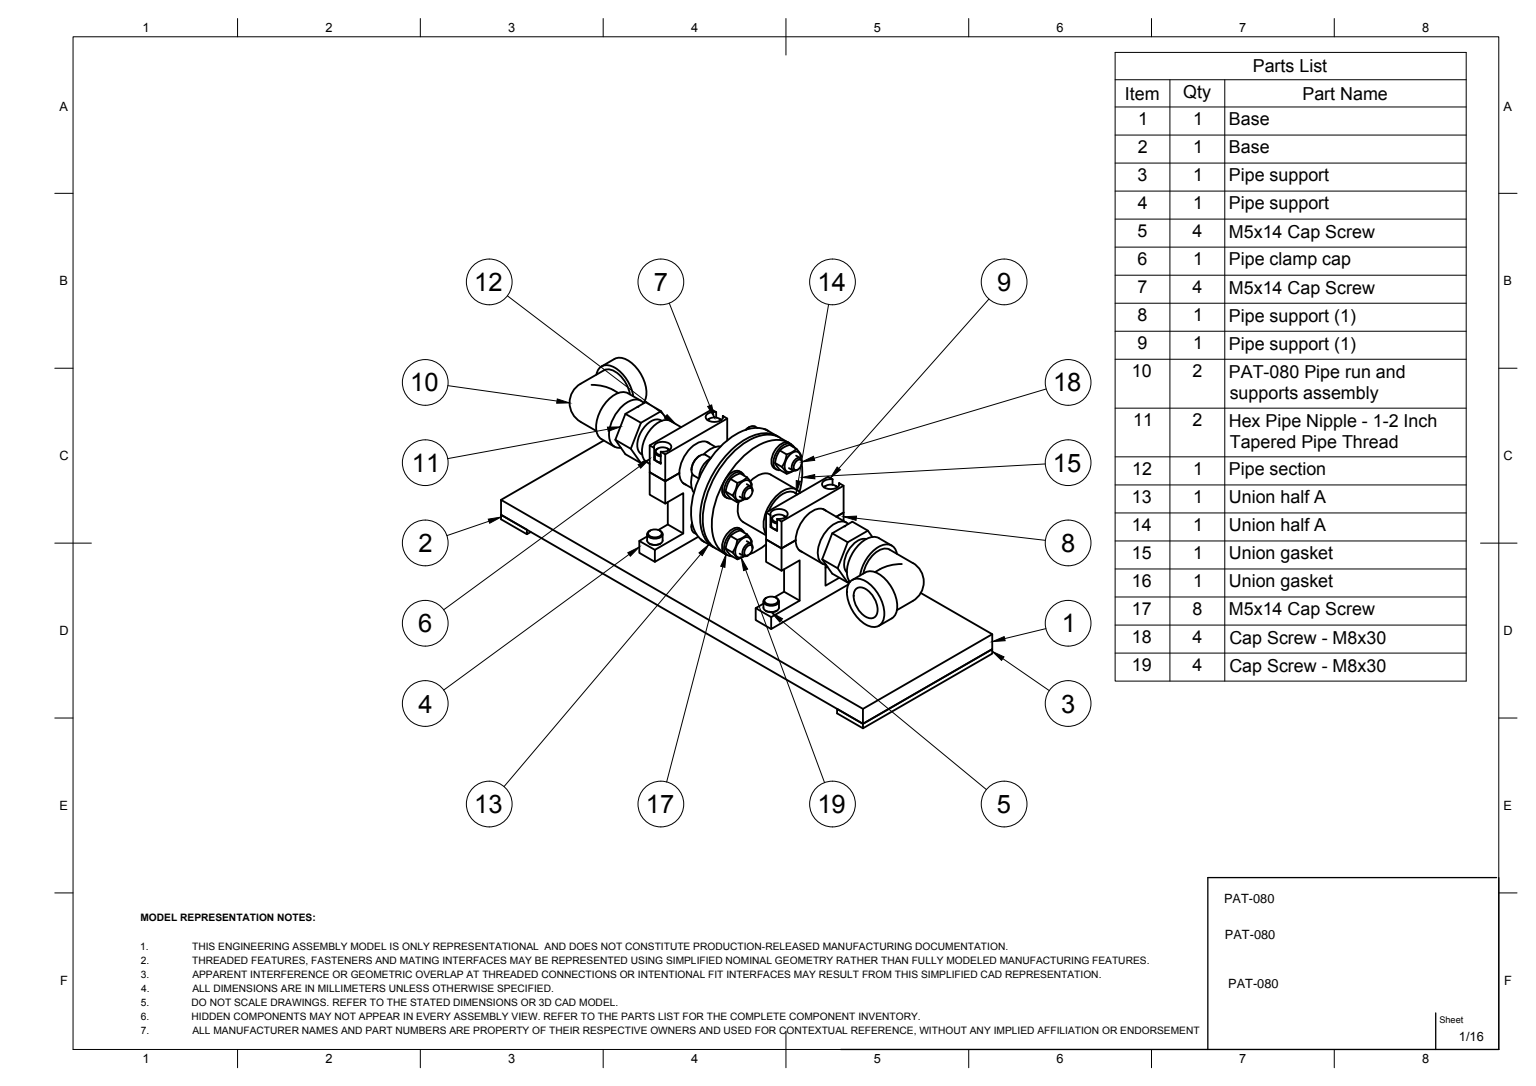
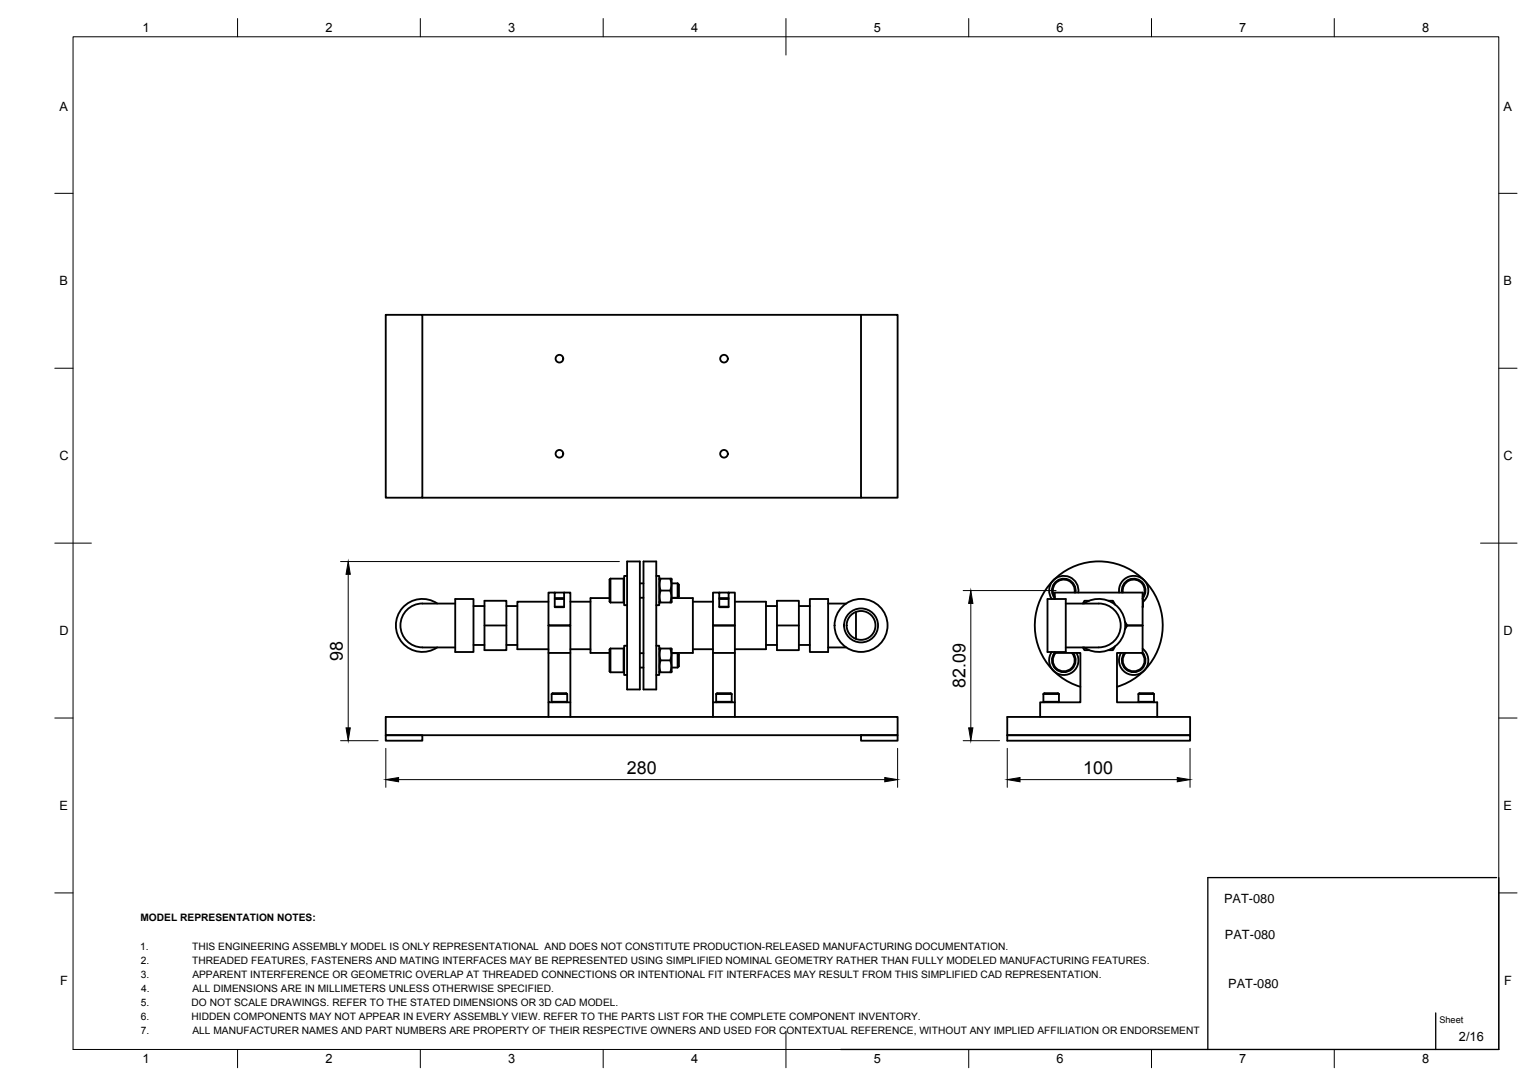
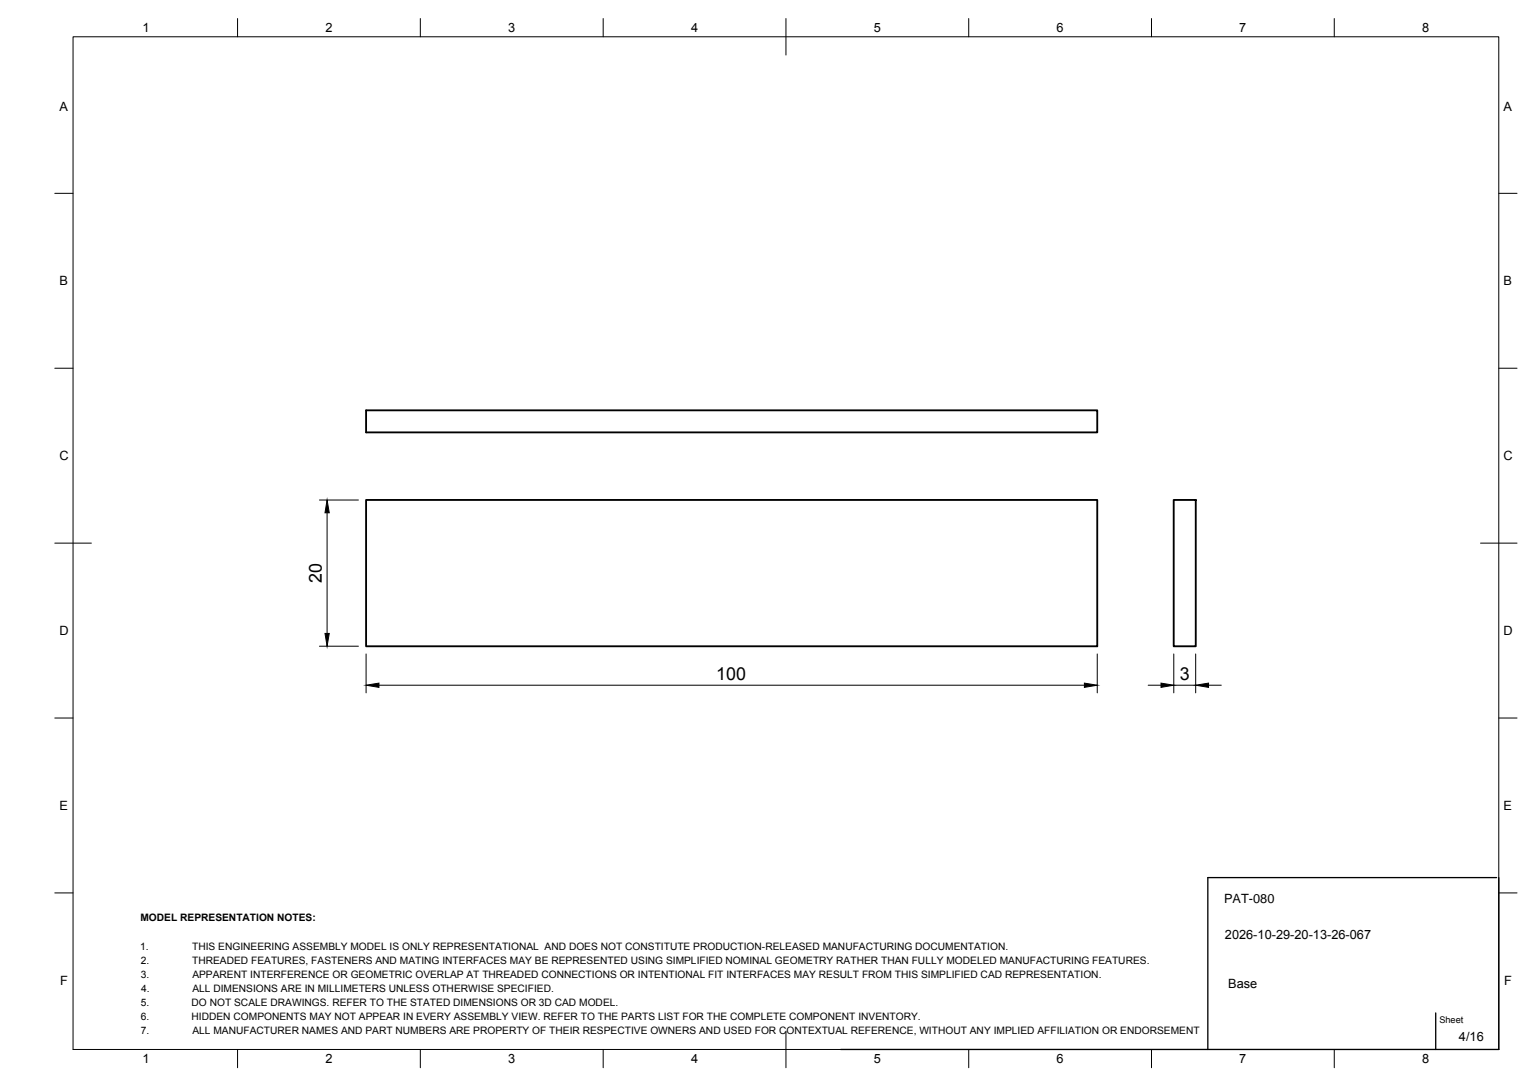
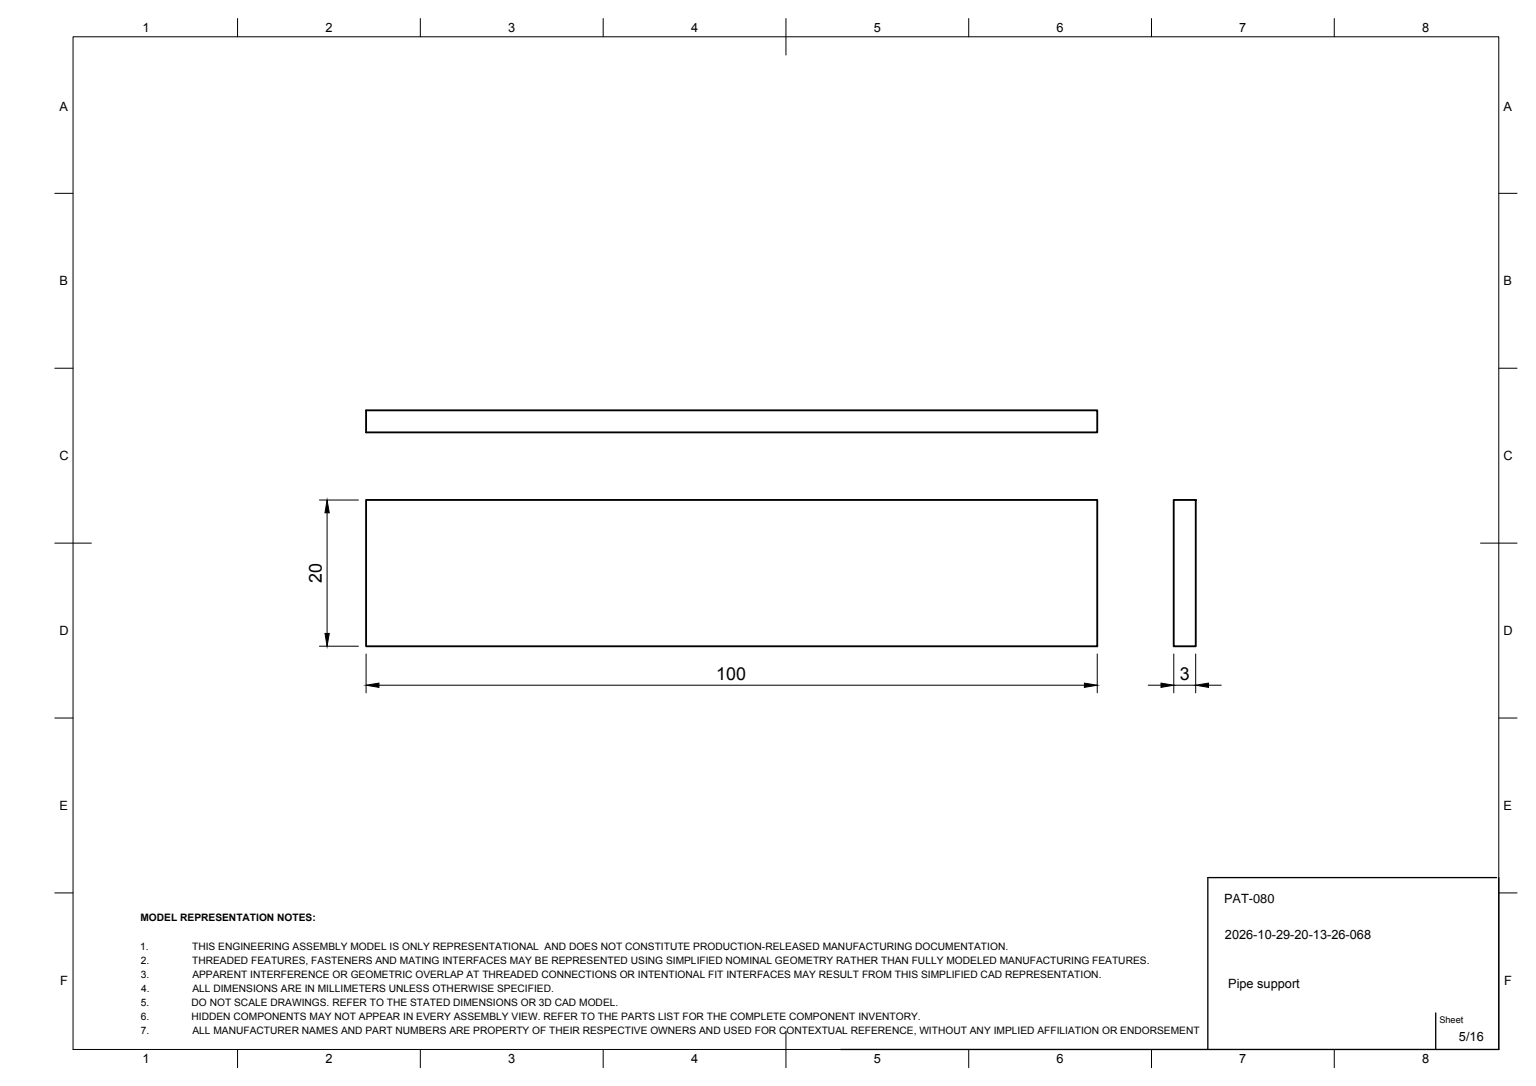
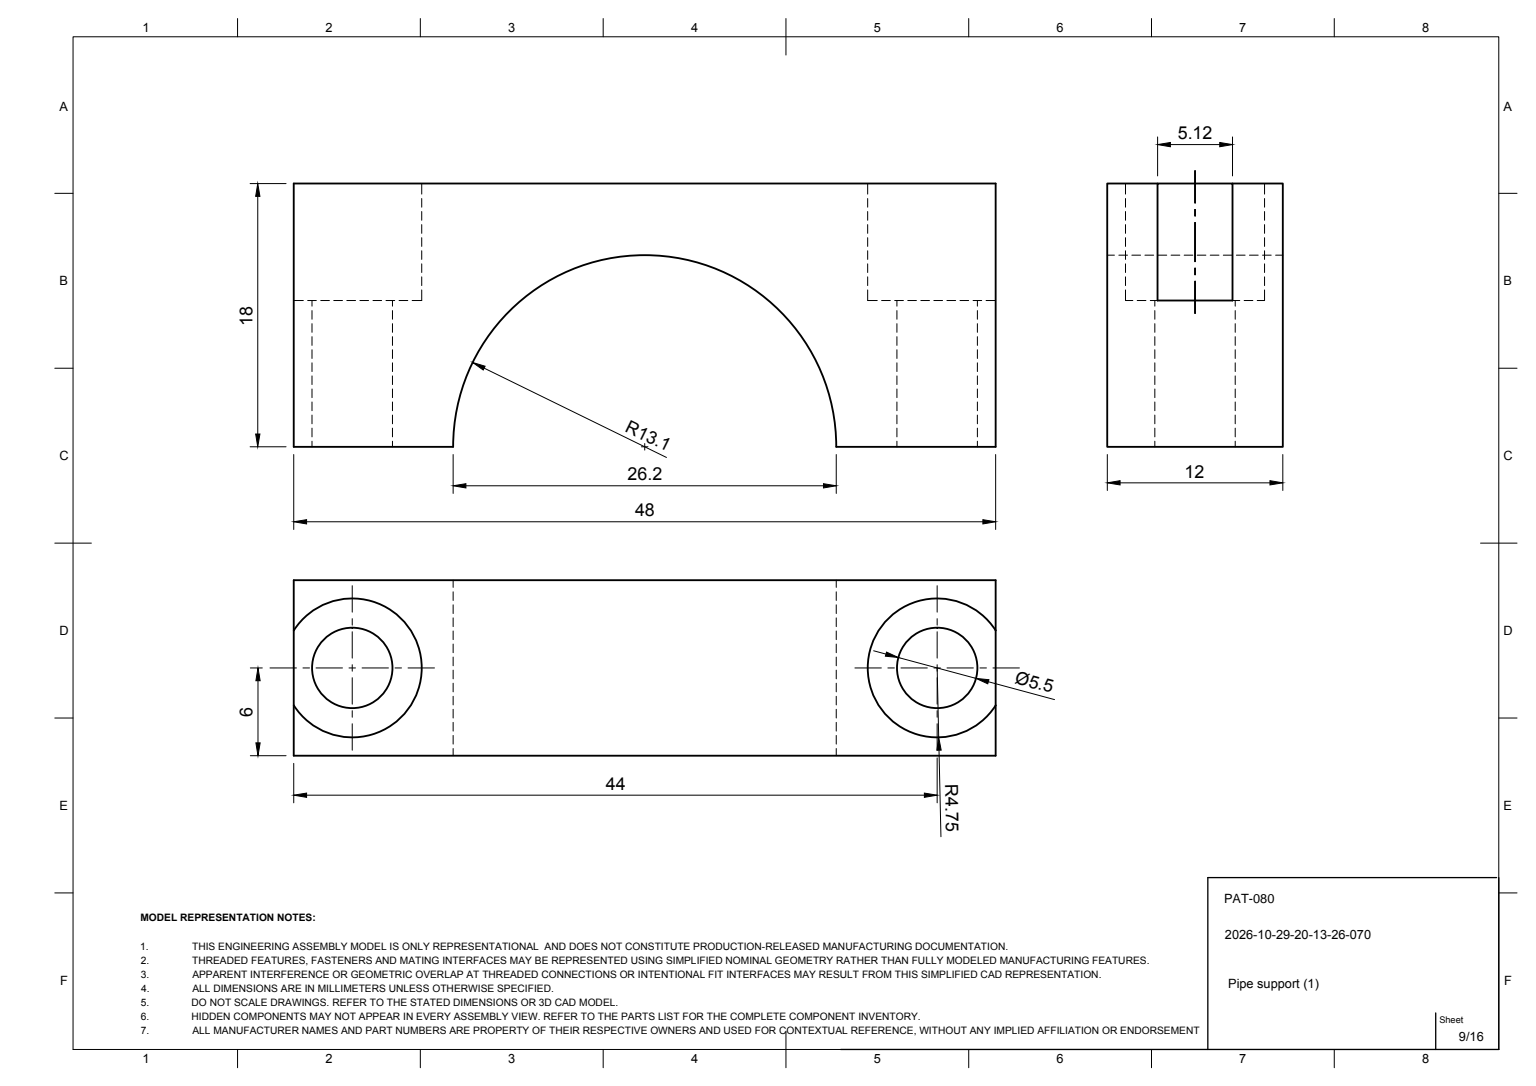
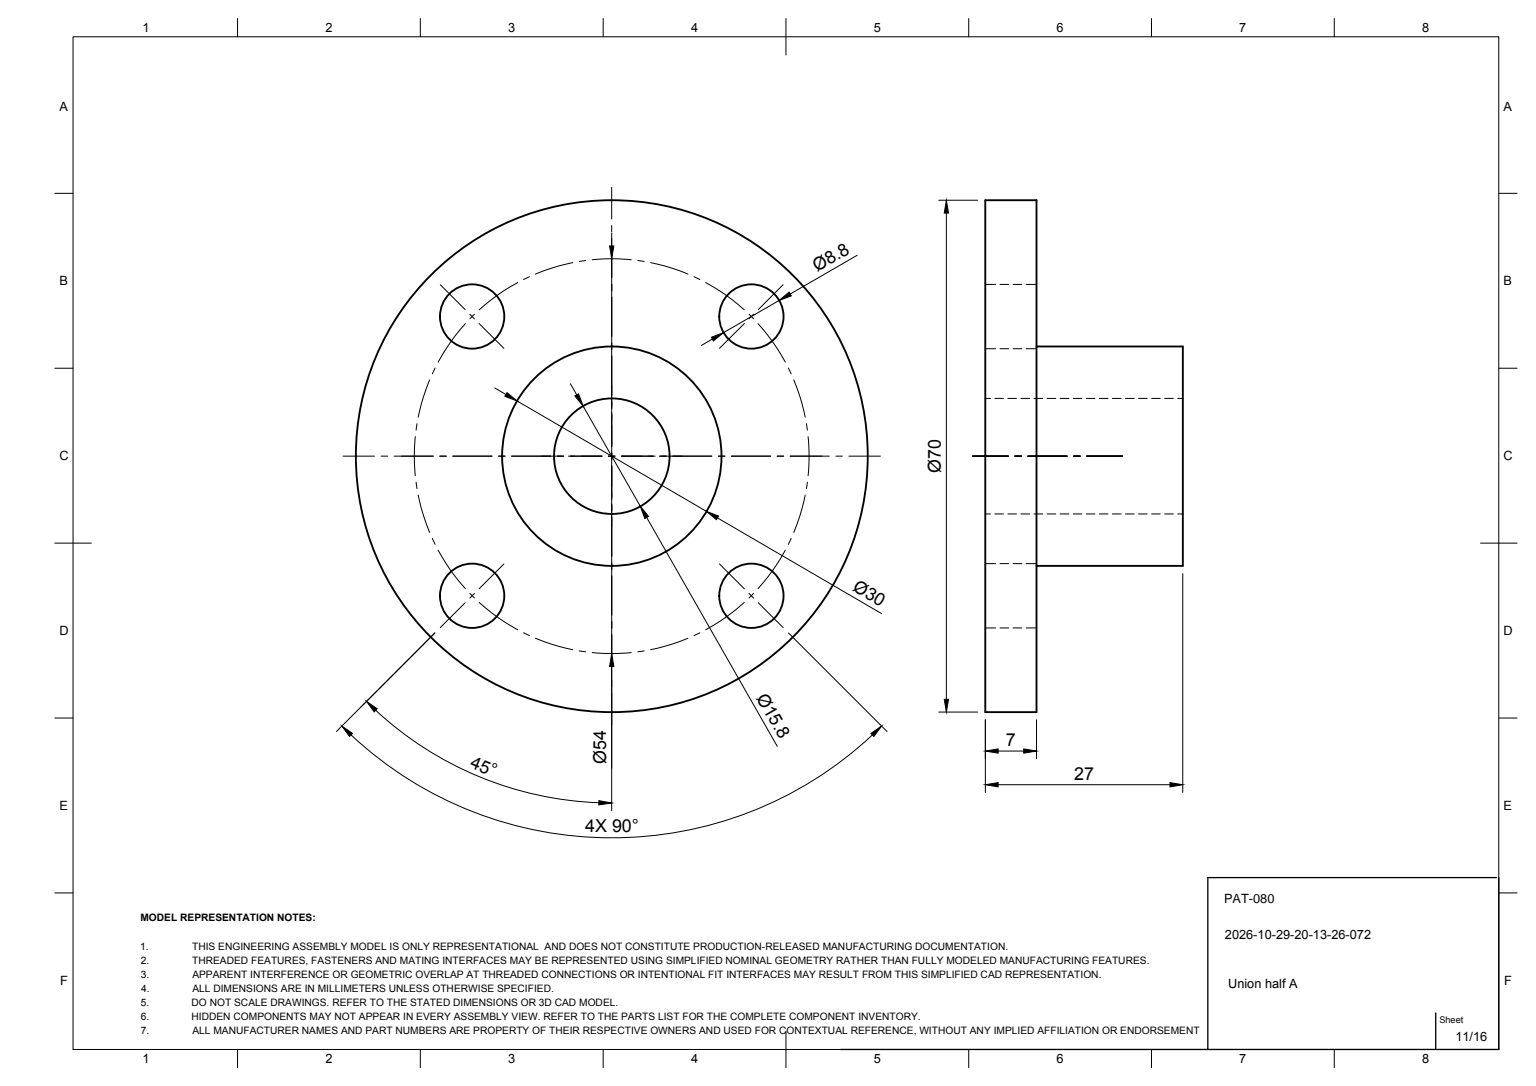
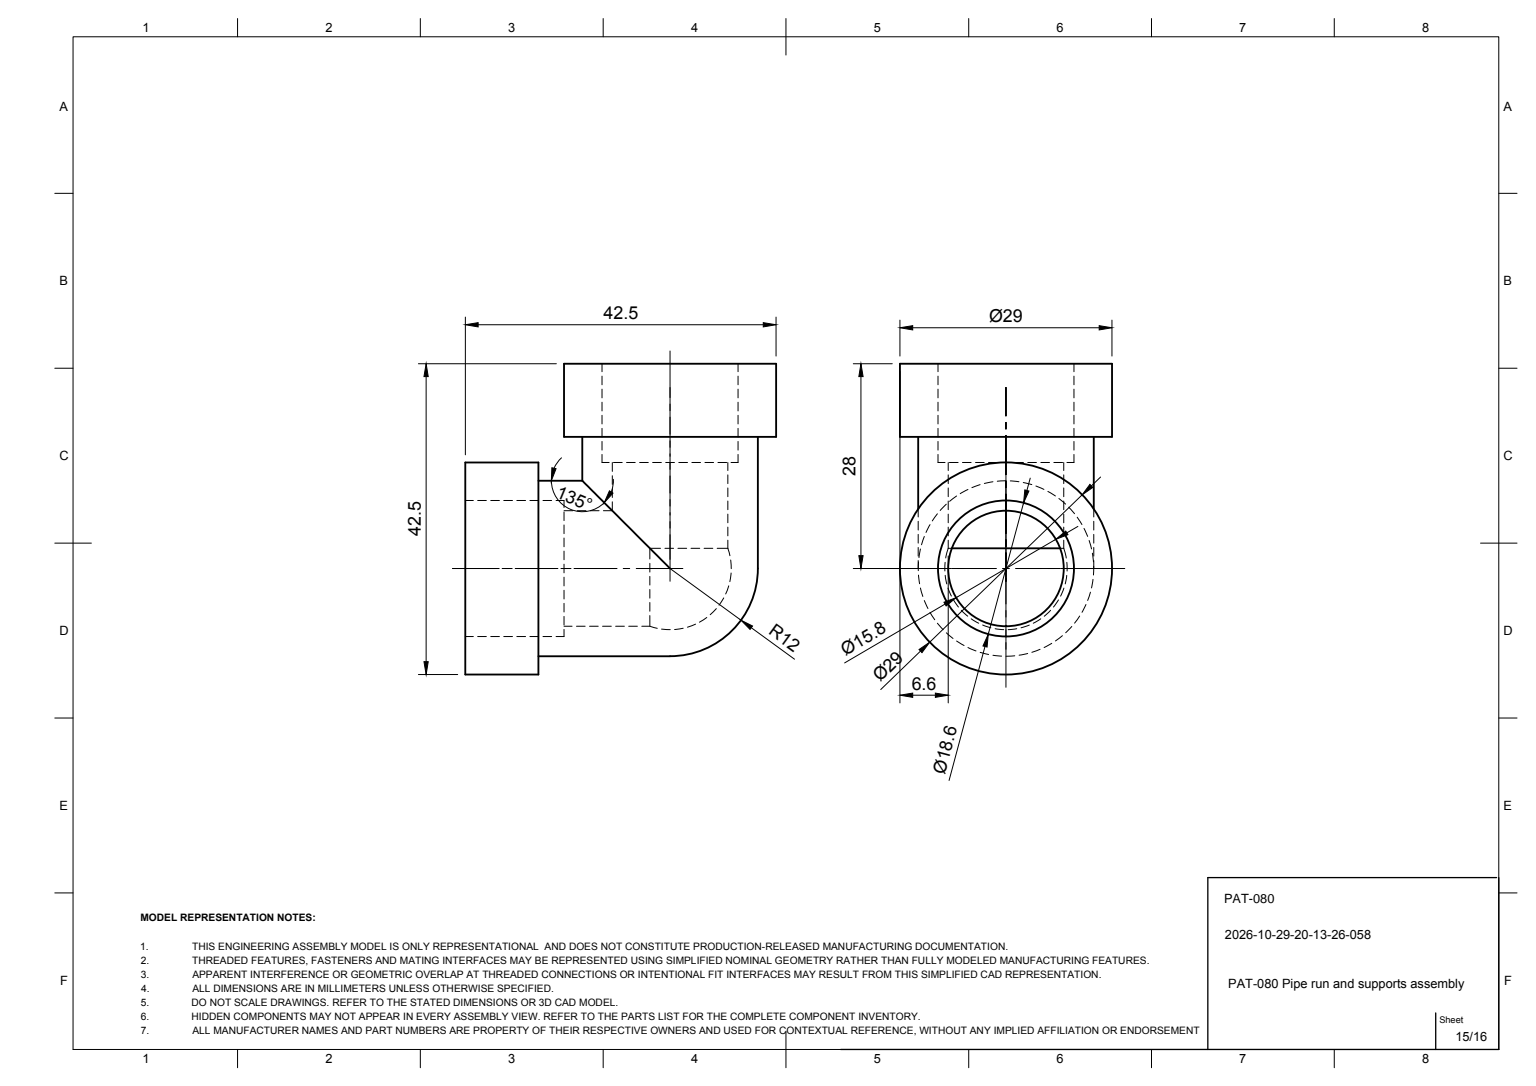
ISO-10303-21;
HEADER;
/* Generated by software containing ST-Developer
 * from STEP Tools, Inc. (www.steptools.com) 
 */

FILE_DESCRIPTION(
/* description */ ('PAT-080'),
/* implementation_level */ '2;1');

FILE_NAME(
/* name */ 'PAT-080',
/* time_stamp */ '2026-10-29T20:13:47-07:00',
/* author */ (''),
/* organization */ (''),
/* preprocessor_version */ 'ST-DEVELOPER v20.2',
/* originating_system */ 'Autodesk Translation Framework v15.17.0.0',
/* authorisation */ '');

FILE_SCHEMA (('AUTOMOTIVE_DESIGN { 1 0 10303 214 3 1 1 }'));
ENDSEC;

DATA;
#10=MECHANICAL_DESIGN_GEOMETRIC_PRESENTATION_REPRESENTATION('',(#246,#247,
#248,#249,#250,#251,#252,#253,#254,#255,#256,#257,#258,#259,#260,#261,#262,
#263,#264),#6878);
#11=ITEM_DEFINED_TRANSFORMATION($,$,#4095,#4494);
#12=ITEM_DEFINED_TRANSFORMATION($,$,#4114,#4495);
#13=ITEM_DEFINED_TRANSFORMATION($,$,#4121,#4496);
#14=ITEM_DEFINED_TRANSFORMATION($,$,#4128,#4497);
#15=ITEM_DEFINED_TRANSFORMATION($,$,#4161,#4498);
#16=ITEM_DEFINED_TRANSFORMATION($,$,#4186,#4499);
#17=ITEM_DEFINED_TRANSFORMATION($,$,#4219,#4500);
#18=ITEM_DEFINED_TRANSFORMATION($,$,#4244,#4501);
#19=ITEM_DEFINED_TRANSFORMATION($,$,#4257,#4502);
#20=ITEM_DEFINED_TRANSFORMATION($,$,#4282,#4503);
#21=ITEM_DEFINED_TRANSFORMATION($,$,#4295,#4504);
#22=ITEM_DEFINED_TRANSFORMATION($,$,#4320,#4505);
#23=ITEM_DEFINED_TRANSFORMATION($,$,#4329,#4506);
#24=ITEM_DEFINED_TRANSFORMATION($,$,#4329,#4507);
#25=ITEM_DEFINED_TRANSFORMATION($,$,#4353,#4508);
#26=ITEM_DEFINED_TRANSFORMATION($,$,#4353,#4509);
#27=ITEM_DEFINED_TRANSFORMATION($,$,#4329,#4510);
#28=ITEM_DEFINED_TRANSFORMATION($,$,#4329,#4511);
#29=ITEM_DEFINED_TRANSFORMATION($,$,#4353,#4512);
#30=ITEM_DEFINED_TRANSFORMATION($,$,#4353,#4513);
#31=ITEM_DEFINED_TRANSFORMATION($,$,#4379,#4514);
#32=ITEM_DEFINED_TRANSFORMATION($,$,#4379,#4515);
#33=ITEM_DEFINED_TRANSFORMATION($,$,#4419,#4516);
#34=ITEM_DEFINED_TRANSFORMATION($,$,#4419,#4517);
#35=ITEM_DEFINED_TRANSFORMATION($,$,#4469,#4518);
#36=ITEM_DEFINED_TRANSFORMATION($,$,#4443,#4519);
#37=ITEM_DEFINED_TRANSFORMATION($,$,#4469,#4520);
#38=ITEM_DEFINED_TRANSFORMATION($,$,#4478,#4521);
#39=ITEM_DEFINED_TRANSFORMATION($,$,#4469,#4522);
#40=ITEM_DEFINED_TRANSFORMATION($,$,#4443,#4523);
#41=ITEM_DEFINED_TRANSFORMATION($,$,#4469,#4524);
#42=ITEM_DEFINED_TRANSFORMATION($,$,#4478,#4525);
#43=ITEM_DEFINED_TRANSFORMATION($,$,#4469,#4526);
#44=ITEM_DEFINED_TRANSFORMATION($,$,#4443,#4527);
#45=ITEM_DEFINED_TRANSFORMATION($,$,#4469,#4528);
#46=ITEM_DEFINED_TRANSFORMATION($,$,#4478,#4529);
#47=ITEM_DEFINED_TRANSFORMATION($,$,#4469,#4530);
#48=ITEM_DEFINED_TRANSFORMATION($,$,#4443,#4531);
#49=ITEM_DEFINED_TRANSFORMATION($,$,#4469,#4532);
#50=ITEM_DEFINED_TRANSFORMATION($,$,#4478,#4533);
#51=(
REPRESENTATION_RELATIONSHIP($,$,#6964,#6963)
REPRESENTATION_RELATIONSHIP_WITH_TRANSFORMATION(#11)
SHAPE_REPRESENTATION_RELATIONSHIP()
);
#52=(
REPRESENTATION_RELATIONSHIP($,$,#6965,#6963)
REPRESENTATION_RELATIONSHIP_WITH_TRANSFORMATION(#12)
SHAPE_REPRESENTATION_RELATIONSHIP()
);
#53=(
REPRESENTATION_RELATIONSHIP($,$,#6966,#6963)
REPRESENTATION_RELATIONSHIP_WITH_TRANSFORMATION(#13)
SHAPE_REPRESENTATION_RELATIONSHIP()
);
#54=(
REPRESENTATION_RELATIONSHIP($,$,#6967,#6963)
REPRESENTATION_RELATIONSHIP_WITH_TRANSFORMATION(#14)
SHAPE_REPRESENTATION_RELATIONSHIP()
);
#55=(
REPRESENTATION_RELATIONSHIP($,$,#6968,#6963)
REPRESENTATION_RELATIONSHIP_WITH_TRANSFORMATION(#15)
SHAPE_REPRESENTATION_RELATIONSHIP()
);
#56=(
REPRESENTATION_RELATIONSHIP($,$,#6969,#6963)
REPRESENTATION_RELATIONSHIP_WITH_TRANSFORMATION(#16)
SHAPE_REPRESENTATION_RELATIONSHIP()
);
#57=(
REPRESENTATION_RELATIONSHIP($,$,#6970,#6963)
REPRESENTATION_RELATIONSHIP_WITH_TRANSFORMATION(#17)
SHAPE_REPRESENTATION_RELATIONSHIP()
);
#58=(
REPRESENTATION_RELATIONSHIP($,$,#6971,#6963)
REPRESENTATION_RELATIONSHIP_WITH_TRANSFORMATION(#18)
SHAPE_REPRESENTATION_RELATIONSHIP()
);
#59=(
REPRESENTATION_RELATIONSHIP($,$,#6972,#6963)
REPRESENTATION_RELATIONSHIP_WITH_TRANSFORMATION(#19)
SHAPE_REPRESENTATION_RELATIONSHIP()
);
#60=(
REPRESENTATION_RELATIONSHIP($,$,#6973,#6963)
REPRESENTATION_RELATIONSHIP_WITH_TRANSFORMATION(#20)
SHAPE_REPRESENTATION_RELATIONSHIP()
);
#61=(
REPRESENTATION_RELATIONSHIP($,$,#6974,#6963)
REPRESENTATION_RELATIONSHIP_WITH_TRANSFORMATION(#21)
SHAPE_REPRESENTATION_RELATIONSHIP()
);
#62=(
REPRESENTATION_RELATIONSHIP($,$,#6975,#6963)
REPRESENTATION_RELATIONSHIP_WITH_TRANSFORMATION(#22)
SHAPE_REPRESENTATION_RELATIONSHIP()
);
#63=(
REPRESENTATION_RELATIONSHIP($,$,#6976,#6963)
REPRESENTATION_RELATIONSHIP_WITH_TRANSFORMATION(#23)
SHAPE_REPRESENTATION_RELATIONSHIP()
);
#64=(
REPRESENTATION_RELATIONSHIP($,$,#6976,#6963)
REPRESENTATION_RELATIONSHIP_WITH_TRANSFORMATION(#24)
SHAPE_REPRESENTATION_RELATIONSHIP()
);
#65=(
REPRESENTATION_RELATIONSHIP($,$,#6977,#6963)
REPRESENTATION_RELATIONSHIP_WITH_TRANSFORMATION(#25)
SHAPE_REPRESENTATION_RELATIONSHIP()
);
#66=(
REPRESENTATION_RELATIONSHIP($,$,#6977,#6963)
REPRESENTATION_RELATIONSHIP_WITH_TRANSFORMATION(#26)
SHAPE_REPRESENTATION_RELATIONSHIP()
);
#67=(
REPRESENTATION_RELATIONSHIP($,$,#6976,#6963)
REPRESENTATION_RELATIONSHIP_WITH_TRANSFORMATION(#27)
SHAPE_REPRESENTATION_RELATIONSHIP()
);
#68=(
REPRESENTATION_RELATIONSHIP($,$,#6976,#6963)
REPRESENTATION_RELATIONSHIP_WITH_TRANSFORMATION(#28)
SHAPE_REPRESENTATION_RELATIONSHIP()
);
#69=(
REPRESENTATION_RELATIONSHIP($,$,#6977,#6963)
REPRESENTATION_RELATIONSHIP_WITH_TRANSFORMATION(#29)
SHAPE_REPRESENTATION_RELATIONSHIP()
);
#70=(
REPRESENTATION_RELATIONSHIP($,$,#6977,#6963)
REPRESENTATION_RELATIONSHIP_WITH_TRANSFORMATION(#30)
SHAPE_REPRESENTATION_RELATIONSHIP()
);
#71=(
REPRESENTATION_RELATIONSHIP($,$,#6978,#6963)
REPRESENTATION_RELATIONSHIP_WITH_TRANSFORMATION(#31)
SHAPE_REPRESENTATION_RELATIONSHIP()
);
#72=(
REPRESENTATION_RELATIONSHIP($,$,#6978,#6963)
REPRESENTATION_RELATIONSHIP_WITH_TRANSFORMATION(#32)
SHAPE_REPRESENTATION_RELATIONSHIP()
);
#73=(
REPRESENTATION_RELATIONSHIP($,$,#6979,#6963)
REPRESENTATION_RELATIONSHIP_WITH_TRANSFORMATION(#33)
SHAPE_REPRESENTATION_RELATIONSHIP()
);
#74=(
REPRESENTATION_RELATIONSHIP($,$,#6979,#6963)
REPRESENTATION_RELATIONSHIP_WITH_TRANSFORMATION(#34)
SHAPE_REPRESENTATION_RELATIONSHIP()
);
#75=(
REPRESENTATION_RELATIONSHIP($,$,#6981,#6963)
REPRESENTATION_RELATIONSHIP_WITH_TRANSFORMATION(#35)
SHAPE_REPRESENTATION_RELATIONSHIP()
);
#76=(
REPRESENTATION_RELATIONSHIP($,$,#6980,#6963)
REPRESENTATION_RELATIONSHIP_WITH_TRANSFORMATION(#36)
SHAPE_REPRESENTATION_RELATIONSHIP()
);
#77=(
REPRESENTATION_RELATIONSHIP($,$,#6981,#6963)
REPRESENTATION_RELATIONSHIP_WITH_TRANSFORMATION(#37)
SHAPE_REPRESENTATION_RELATIONSHIP()
);
#78=(
REPRESENTATION_RELATIONSHIP($,$,#6982,#6963)
REPRESENTATION_RELATIONSHIP_WITH_TRANSFORMATION(#38)
SHAPE_REPRESENTATION_RELATIONSHIP()
);
#79=(
REPRESENTATION_RELATIONSHIP($,$,#6981,#6963)
REPRESENTATION_RELATIONSHIP_WITH_TRANSFORMATION(#39)
SHAPE_REPRESENTATION_RELATIONSHIP()
);
#80=(
REPRESENTATION_RELATIONSHIP($,$,#6980,#6963)
REPRESENTATION_RELATIONSHIP_WITH_TRANSFORMATION(#40)
SHAPE_REPRESENTATION_RELATIONSHIP()
);
#81=(
REPRESENTATION_RELATIONSHIP($,$,#6981,#6963)
REPRESENTATION_RELATIONSHIP_WITH_TRANSFORMATION(#41)
SHAPE_REPRESENTATION_RELATIONSHIP()
);
#82=(
REPRESENTATION_RELATIONSHIP($,$,#6982,#6963)
REPRESENTATION_RELATIONSHIP_WITH_TRANSFORMATION(#42)
SHAPE_REPRESENTATION_RELATIONSHIP()
);
#83=(
REPRESENTATION_RELATIONSHIP($,$,#6981,#6963)
REPRESENTATION_RELATIONSHIP_WITH_TRANSFORMATION(#43)
SHAPE_REPRESENTATION_RELATIONSHIP()
);
#84=(
REPRESENTATION_RELATIONSHIP($,$,#6980,#6963)
REPRESENTATION_RELATIONSHIP_WITH_TRANSFORMATION(#44)
SHAPE_REPRESENTATION_RELATIONSHIP()
);
#85=(
REPRESENTATION_RELATIONSHIP($,$,#6981,#6963)
REPRESENTATION_RELATIONSHIP_WITH_TRANSFORMATION(#45)
SHAPE_REPRESENTATION_RELATIONSHIP()
);
#86=(
REPRESENTATION_RELATIONSHIP($,$,#6982,#6963)
REPRESENTATION_RELATIONSHIP_WITH_TRANSFORMATION(#46)
SHAPE_REPRESENTATION_RELATIONSHIP()
);
#87=(
REPRESENTATION_RELATIONSHIP($,$,#6981,#6963)
REPRESENTATION_RELATIONSHIP_WITH_TRANSFORMATION(#47)
SHAPE_REPRESENTATION_RELATIONSHIP()
);
#88=(
REPRESENTATION_RELATIONSHIP($,$,#6980,#6963)
REPRESENTATION_RELATIONSHIP_WITH_TRANSFORMATION(#48)
SHAPE_REPRESENTATION_RELATIONSHIP()
);
#89=(
REPRESENTATION_RELATIONSHIP($,$,#6981,#6963)
REPRESENTATION_RELATIONSHIP_WITH_TRANSFORMATION(#49)
SHAPE_REPRESENTATION_RELATIONSHIP()
);
#90=(
REPRESENTATION_RELATIONSHIP($,$,#6982,#6963)
REPRESENTATION_RELATIONSHIP_WITH_TRANSFORMATION(#50)
SHAPE_REPRESENTATION_RELATIONSHIP()
);
#91=CONTEXT_DEPENDENT_SHAPE_REPRESENTATION(#51,#6923);
#92=CONTEXT_DEPENDENT_SHAPE_REPRESENTATION(#52,#6924);
#93=CONTEXT_DEPENDENT_SHAPE_REPRESENTATION(#53,#6925);
#94=CONTEXT_DEPENDENT_SHAPE_REPRESENTATION(#54,#6926);
#95=CONTEXT_DEPENDENT_SHAPE_REPRESENTATION(#55,#6927);
#96=CONTEXT_DEPENDENT_SHAPE_REPRESENTATION(#56,#6928);
#97=CONTEXT_DEPENDENT_SHAPE_REPRESENTATION(#57,#6929);
#98=CONTEXT_DEPENDENT_SHAPE_REPRESENTATION(#58,#6930);
#99=CONTEXT_DEPENDENT_SHAPE_REPRESENTATION(#59,#6931);
#100=CONTEXT_DEPENDENT_SHAPE_REPRESENTATION(#60,#6932);
#101=CONTEXT_DEPENDENT_SHAPE_REPRESENTATION(#61,#6933);
#102=CONTEXT_DEPENDENT_SHAPE_REPRESENTATION(#62,#6934);
#103=CONTEXT_DEPENDENT_SHAPE_REPRESENTATION(#63,#6935);
#104=CONTEXT_DEPENDENT_SHAPE_REPRESENTATION(#64,#6936);
#105=CONTEXT_DEPENDENT_SHAPE_REPRESENTATION(#65,#6937);
#106=CONTEXT_DEPENDENT_SHAPE_REPRESENTATION(#66,#6938);
#107=CONTEXT_DEPENDENT_SHAPE_REPRESENTATION(#67,#6939);
#108=CONTEXT_DEPENDENT_SHAPE_REPRESENTATION(#68,#6940);
#109=CONTEXT_DEPENDENT_SHAPE_REPRESENTATION(#69,#6941);
#110=CONTEXT_DEPENDENT_SHAPE_REPRESENTATION(#70,#6942);
#111=CONTEXT_DEPENDENT_SHAPE_REPRESENTATION(#71,#6943);
#112=CONTEXT_DEPENDENT_SHAPE_REPRESENTATION(#72,#6944);
#113=CONTEXT_DEPENDENT_SHAPE_REPRESENTATION(#73,#6945);
#114=CONTEXT_DEPENDENT_SHAPE_REPRESENTATION(#74,#6946);
#115=CONTEXT_DEPENDENT_SHAPE_REPRESENTATION(#75,#6947);
#116=CONTEXT_DEPENDENT_SHAPE_REPRESENTATION(#76,#6948);
#117=CONTEXT_DEPENDENT_SHAPE_REPRESENTATION(#77,#6949);
#118=CONTEXT_DEPENDENT_SHAPE_REPRESENTATION(#78,#6950);
#119=CONTEXT_DEPENDENT_SHAPE_REPRESENTATION(#79,#6951);
#120=CONTEXT_DEPENDENT_SHAPE_REPRESENTATION(#80,#6952);
#121=CONTEXT_DEPENDENT_SHAPE_REPRESENTATION(#81,#6953);
#122=CONTEXT_DEPENDENT_SHAPE_REPRESENTATION(#82,#6954);
#123=CONTEXT_DEPENDENT_SHAPE_REPRESENTATION(#83,#6955);
#124=CONTEXT_DEPENDENT_SHAPE_REPRESENTATION(#84,#6956);
#125=CONTEXT_DEPENDENT_SHAPE_REPRESENTATION(#85,#6957);
#126=CONTEXT_DEPENDENT_SHAPE_REPRESENTATION(#86,#6958);
#127=CONTEXT_DEPENDENT_SHAPE_REPRESENTATION(#87,#6959);
#128=CONTEXT_DEPENDENT_SHAPE_REPRESENTATION(#88,#6960);
#129=CONTEXT_DEPENDENT_SHAPE_REPRESENTATION(#89,#6961);
#130=CONTEXT_DEPENDENT_SHAPE_REPRESENTATION(#90,#6962);
#131=NEXT_ASSEMBLY_USAGE_OCCURRENCE('Base:1','Base:1','Base:1',#6984,#6985,
'Base:1');
#132=NEXT_ASSEMBLY_USAGE_OCCURRENCE('Bonded pad:1','Bonded pad:1',
'Bonded pad:1',#6984,#6986,'Bonded pad:1');
#133=NEXT_ASSEMBLY_USAGE_OCCURRENCE('Bonded pad (1):1',
'Bonded pad (1):1','Bonded pad (1):1',#6984,#6987,'Bonded pad (1):1');
#134=NEXT_ASSEMBLY_USAGE_OCCURRENCE('Pipe support:1','Pipe support:1',
'Pipe support:1',#6984,#6988,'Pipe support:1');
#135=NEXT_ASSEMBLY_USAGE_OCCURRENCE('Pipe clamp cap:1',
'Pipe clamp cap:1','Pipe clamp cap:1',#6984,#6989,'Pipe clamp cap:1');
#136=NEXT_ASSEMBLY_USAGE_OCCURRENCE('Pipe support (1):1',
'Pipe support (1):1','Pipe support (1):1',#6984,#6990,
'Pipe support (1):1');
#137=NEXT_ASSEMBLY_USAGE_OCCURRENCE('Pipe clamp cap (1):1',
'Pipe clamp cap (1):1','Pipe clamp cap (1):1',#6984,#6991,
'Pipe clamp cap (1):1');
#138=NEXT_ASSEMBLY_USAGE_OCCURRENCE('Pipe section:1','Pipe section:1',
'Pipe section:1',#6984,#6992,'Pipe section:1');
#139=NEXT_ASSEMBLY_USAGE_OCCURRENCE('Union half A:1','Union half A:1',
'Union half A:1',#6984,#6993,'Union half A:1');
#140=NEXT_ASSEMBLY_USAGE_OCCURRENCE('Pipe section (1):1',
'Pipe section (1):1','Pipe section (1):1',#6984,#6994,
'Pipe section (1):1');
#141=NEXT_ASSEMBLY_USAGE_OCCURRENCE('Union half B:1','Union half B:1',
'Union half B:1',#6984,#6995,'Union half B:1');
#142=NEXT_ASSEMBLY_USAGE_OCCURRENCE('Union gasket:1','Union gasket:1',
'Union gasket:1',#6984,#6996,'Union gasket:1');
#143=NEXT_ASSEMBLY_USAGE_OCCURRENCE('M5x14 Cap Screw:1',
'M5x14 Cap Screw:1','M5x14 Cap Screw:1',#6984,#6997,'M5x14 Cap Screw:1');
#144=NEXT_ASSEMBLY_USAGE_OCCURRENCE('M5x14 Cap Screw:2',
'M5x14 Cap Screw:2','M5x14 Cap Screw:2',#6984,#6997,'M5x14 Cap Screw:2');
#145=NEXT_ASSEMBLY_USAGE_OCCURRENCE('Cap Screw - M5x20:1',
'Cap Screw - M5x20:1','Cap Screw - M5x20:1',#6984,#6998,
'Cap Screw - M5x20:1');
#146=NEXT_ASSEMBLY_USAGE_OCCURRENCE('Cap Screw - M5x20:2',
'Cap Screw - M5x20:2','Cap Screw - M5x20:2',#6984,#6998,
'Cap Screw - M5x20:2');
#147=NEXT_ASSEMBLY_USAGE_OCCURRENCE('M5x14 Cap Screw:3',
'M5x14 Cap Screw:3','M5x14 Cap Screw:3',#6984,#6997,'M5x14 Cap Screw:3');
#148=NEXT_ASSEMBLY_USAGE_OCCURRENCE('M5x14 Cap Screw:4',
'M5x14 Cap Screw:4','M5x14 Cap Screw:4',#6984,#6997,'M5x14 Cap Screw:4');
#149=NEXT_ASSEMBLY_USAGE_OCCURRENCE('Cap Screw - M5x20:3',
'Cap Screw - M5x20:3','Cap Screw - M5x20:3',#6984,#6998,
'Cap Screw - M5x20:3');
#150=NEXT_ASSEMBLY_USAGE_OCCURRENCE('Cap Screw - M5x20:4',
'Cap Screw - M5x20:4','Cap Screw - M5x20:4',#6984,#6998,
'Cap Screw - M5x20:4');
#151=NEXT_ASSEMBLY_USAGE_OCCURRENCE(
'Pipe Elbow - 90 Degrees, 1-2 Inch Tapered Pipe Thread:1',
'Pipe Elbow - 90 Degrees, 1-2 Inch Tapered Pipe Thread:1',
'Pipe Elbow - 90 Degrees, 1-2 Inch Tapered Pipe Thread:1',#6984,#6999,
'Pipe Elbow - 90 Degrees, 1-2 Inch Tapered Pipe Thread:1');
#152=NEXT_ASSEMBLY_USAGE_OCCURRENCE(
'Pipe Elbow - 90 Degrees, 1-2 Inch Tapered Pipe Thread:2',
'Pipe Elbow - 90 Degrees, 1-2 Inch Tapered Pipe Thread:2',
'Pipe Elbow - 90 Degrees, 1-2 Inch Tapered Pipe Thread:2',#6984,#6999,
'Pipe Elbow - 90 Degrees, 1-2 Inch Tapered Pipe Thread:2');
#153=NEXT_ASSEMBLY_USAGE_OCCURRENCE(
'Hex Pipe Nipple - 1-2 Inch Tapered Pipe Thread:1',
'Hex Pipe Nipple - 1-2 Inch Tapered Pipe Thread:1',
'Hex Pipe Nipple - 1-2 Inch Tapered Pipe Thread:1',#6984,#7000,
'Hex Pipe Nipple - 1-2 Inch Tapered Pipe Thread:1');
#154=NEXT_ASSEMBLY_USAGE_OCCURRENCE(
'Hex Pipe Nipple - 1-2 Inch Tapered Pipe Thread:2',
'Hex Pipe Nipple - 1-2 Inch Tapered Pipe Thread:2',
'Hex Pipe Nipple - 1-2 Inch Tapered Pipe Thread:2',#6984,#7000,
'Hex Pipe Nipple - 1-2 Inch Tapered Pipe Thread:2');
#155=NEXT_ASSEMBLY_USAGE_OCCURRENCE('Flat Washer - M8:1',
'Flat Washer - M8:1','Flat Washer - M8:1',#6984,#7002,
'Flat Washer - M8:1');
#156=NEXT_ASSEMBLY_USAGE_OCCURRENCE('Cap Screw - M8x30:1',
'Cap Screw - M8x30:1','Cap Screw - M8x30:1',#6984,#7001,
'Cap Screw - M8x30:1');
#157=NEXT_ASSEMBLY_USAGE_OCCURRENCE('Flat Washer - M8:2',
'Flat Washer - M8:2','Flat Washer - M8:2',#6984,#7002,
'Flat Washer - M8:2');
#158=NEXT_ASSEMBLY_USAGE_OCCURRENCE('Hex Nut - M8:1','Hex Nut - M8:1',
'Hex Nut - M8:1',#6984,#7003,'Hex Nut - M8:1');
#159=NEXT_ASSEMBLY_USAGE_OCCURRENCE('Flat Washer - M8:3',
'Flat Washer - M8:3','Flat Washer - M8:3',#6984,#7002,
'Flat Washer - M8:3');
#160=NEXT_ASSEMBLY_USAGE_OCCURRENCE('Cap Screw - M8x30:2',
'Cap Screw - M8x30:2','Cap Screw - M8x30:2',#6984,#7001,
'Cap Screw - M8x30:2');
#161=NEXT_ASSEMBLY_USAGE_OCCURRENCE('Flat Washer - M8:4',
'Flat Washer - M8:4','Flat Washer - M8:4',#6984,#7002,
'Flat Washer - M8:4');
#162=NEXT_ASSEMBLY_USAGE_OCCURRENCE('Hex Nut - M8:2','Hex Nut - M8:2',
'Hex Nut - M8:2',#6984,#7003,'Hex Nut - M8:2');
#163=NEXT_ASSEMBLY_USAGE_OCCURRENCE('Flat Washer - M8:5',
'Flat Washer - M8:5','Flat Washer - M8:5',#6984,#7002,
'Flat Washer - M8:5');
#164=NEXT_ASSEMBLY_USAGE_OCCURRENCE('Cap Screw - M8x30:3',
'Cap Screw - M8x30:3','Cap Screw - M8x30:3',#6984,#7001,
'Cap Screw - M8x30:3');
#165=NEXT_ASSEMBLY_USAGE_OCCURRENCE('Flat Washer - M8:6',
'Flat Washer - M8:6','Flat Washer - M8:6',#6984,#7002,
'Flat Washer - M8:6');
#166=NEXT_ASSEMBLY_USAGE_OCCURRENCE('Hex Nut - M8:3','Hex Nut - M8:3',
'Hex Nut - M8:3',#6984,#7003,'Hex Nut - M8:3');
#167=NEXT_ASSEMBLY_USAGE_OCCURRENCE('Flat Washer - M8:7',
'Flat Washer - M8:7','Flat Washer - M8:7',#6984,#7002,
'Flat Washer - M8:7');
#168=NEXT_ASSEMBLY_USAGE_OCCURRENCE('Cap Screw - M8x30:4',
'Cap Screw - M8x30:4','Cap Screw - M8x30:4',#6984,#7001,
'Cap Screw - M8x30:4');
#169=NEXT_ASSEMBLY_USAGE_OCCURRENCE('Flat Washer - M8:8',
'Flat Washer - M8:8','Flat Washer - M8:8',#6984,#7002,
'Flat Washer - M8:8');
#170=NEXT_ASSEMBLY_USAGE_OCCURRENCE('Hex Nut - M8:4','Hex Nut - M8:4',
'Hex Nut - M8:4',#6984,#7003,'Hex Nut - M8:4');
#171=(
BOUNDED_CURVE()
B_SPLINE_CURVE(2,(#6724,#6725,#6726),.UNSPECIFIED.,.F.,.F.)
B_SPLINE_CURVE_WITH_KNOTS((3,3),(0.14973948338295,0.97160236658079),
 .UNSPECIFIED.)
CURVE()
GEOMETRIC_REPRESENTATION_ITEM()
RATIONAL_B_SPLINE_CURVE((1.07140024848292,1.23714644374248,1.07140024848292))
REPRESENTATION_ITEM('')
);
#172=(
BOUNDED_CURVE()
B_SPLINE_CURVE(2,(#6728,#6729,#6730),.UNSPECIFIED.,.F.,.F.)
B_SPLINE_CURVE_WITH_KNOTS((3,3),(0.14973948338295,0.971602366580789),
 .UNSPECIFIED.)
CURVE()
GEOMETRIC_REPRESENTATION_ITEM()
RATIONAL_B_SPLINE_CURVE((1.07140024848292,1.23714644374248,1.07140024848292))
REPRESENTATION_ITEM('')
);
#173=(
BOUNDED_CURVE()
B_SPLINE_CURVE(2,(#6735,#6736,#6737),.UNSPECIFIED.,.F.,.F.)
B_SPLINE_CURVE_WITH_KNOTS((3,3),(0.14973948338295,0.97160236658079),
 .UNSPECIFIED.)
CURVE()
GEOMETRIC_REPRESENTATION_ITEM()
RATIONAL_B_SPLINE_CURVE((1.07140024848292,1.23714644374248,1.07140024848292))
REPRESENTATION_ITEM('')
);
#174=(
BOUNDED_CURVE()
B_SPLINE_CURVE(2,(#6739,#6740,#6741),.UNSPECIFIED.,.F.,.F.)
B_SPLINE_CURVE_WITH_KNOTS((3,3),(0.14973948338295,0.97160236658079),
 .UNSPECIFIED.)
CURVE()
GEOMETRIC_REPRESENTATION_ITEM()
RATIONAL_B_SPLINE_CURVE((1.07140024848292,1.23714644374248,1.07140024848292))
REPRESENTATION_ITEM('')
);
#175=(
BOUNDED_CURVE()
B_SPLINE_CURVE(2,(#6743,#6744,#6745),.UNSPECIFIED.,.F.,.F.)
B_SPLINE_CURVE_WITH_KNOTS((3,3),(0.14973948338295,0.971602366580789),
 .UNSPECIFIED.)
CURVE()
GEOMETRIC_REPRESENTATION_ITEM()
RATIONAL_B_SPLINE_CURVE((1.07140024848292,1.23714644374248,1.07140024848292))
REPRESENTATION_ITEM('')
);
#176=(
BOUNDED_CURVE()
B_SPLINE_CURVE(2,(#6746,#6747,#6748),.UNSPECIFIED.,.F.,.F.)
B_SPLINE_CURVE_WITH_KNOTS((3,3),(0.14973948338295,0.97160236658079),
 .UNSPECIFIED.)
CURVE()
GEOMETRIC_REPRESENTATION_ITEM()
RATIONAL_B_SPLINE_CURVE((1.07140024848292,1.23714644374248,1.07140024848292))
REPRESENTATION_ITEM('')
);
#177=(
BOUNDED_CURVE()
B_SPLINE_CURVE(2,(#6755,#6756,#6757),.UNSPECIFIED.,.F.,.F.)
B_SPLINE_CURVE_WITH_KNOTS((3,3),(0.14973948338295,0.97160236658079),
 .UNSPECIFIED.)
CURVE()
GEOMETRIC_REPRESENTATION_ITEM()
RATIONAL_B_SPLINE_CURVE((1.07140024848292,1.23714644374248,1.07140024848292))
REPRESENTATION_ITEM('')
);
#178=(
BOUNDED_CURVE()
B_SPLINE_CURVE(2,(#6759,#6760,#6761),.UNSPECIFIED.,.F.,.F.)
B_SPLINE_CURVE_WITH_KNOTS((3,3),(0.14973948338295,0.97160236658079),
 .UNSPECIFIED.)
CURVE()
GEOMETRIC_REPRESENTATION_ITEM()
RATIONAL_B_SPLINE_CURVE((1.07140024848292,1.23714644374248,1.07140024848292))
REPRESENTATION_ITEM('')
);
#179=(
BOUNDED_CURVE()
B_SPLINE_CURVE(2,(#6763,#6764,#6765),.UNSPECIFIED.,.F.,.F.)
B_SPLINE_CURVE_WITH_KNOTS((3,3),(0.14973948338295,0.971602366580789),
 .UNSPECIFIED.)
CURVE()
GEOMETRIC_REPRESENTATION_ITEM()
RATIONAL_B_SPLINE_CURVE((1.07140024848292,1.23714644374248,1.07140024848292))
REPRESENTATION_ITEM('')
);
#180=(
BOUNDED_CURVE()
B_SPLINE_CURVE(2,(#6767,#6768,#6769),.UNSPECIFIED.,.F.,.F.)
B_SPLINE_CURVE_WITH_KNOTS((3,3),(0.14973948338295,0.97160236658079),
 .UNSPECIFIED.)
CURVE()
GEOMETRIC_REPRESENTATION_ITEM()
RATIONAL_B_SPLINE_CURVE((1.07140024848292,1.23714644374248,1.07140024848292))
REPRESENTATION_ITEM('')
);
#181=(
BOUNDED_CURVE()
B_SPLINE_CURVE(2,(#6771,#6772,#6773),.UNSPECIFIED.,.F.,.F.)
B_SPLINE_CURVE_WITH_KNOTS((3,3),(0.14973948338295,0.97160236658079),
 .UNSPECIFIED.)
CURVE()
GEOMETRIC_REPRESENTATION_ITEM()
RATIONAL_B_SPLINE_CURVE((1.07140024848292,1.23714644374248,1.07140024848292))
REPRESENTATION_ITEM('')
);
#182=(
BOUNDED_CURVE()
B_SPLINE_CURVE(2,(#6774,#6775,#6776),.UNSPECIFIED.,.F.,.F.)
B_SPLINE_CURVE_WITH_KNOTS((3,3),(0.14973948338295,0.971602366580789),
 .UNSPECIFIED.)
CURVE()
GEOMETRIC_REPRESENTATION_ITEM()
RATIONAL_B_SPLINE_CURVE((1.07140024848292,1.23714644374248,1.07140024848292))
REPRESENTATION_ITEM('')
);
#183=SPHERICAL_SURFACE('',#4385,0.837);
#184=SPHERICAL_SURFACE('',#4399,1.2);
#185=ELLIPSE('',#4381,1.11722871427475,0.79);
#186=ELLIPSE('',#4405,1.69705627484771,1.2);
#187=CONICAL_SURFACE('',#4342,0.4,0.785398163397448);
#188=CONICAL_SURFACE('',#4346,0.41,0.785398163397448);
#189=CONICAL_SURFACE('',#4350,0.26,0.463647609000806);
#190=CONICAL_SURFACE('',#4356,0.4,0.785398163397448);
#191=CONICAL_SURFACE('',#4360,0.41,0.785398163397448);
#192=CONICAL_SURFACE('',#4364,0.26,0.463647609000806);
#193=CONICAL_SURFACE('',#4368,0.225,0.785398163397448);
#194=CONICAL_SURFACE('',#4435,1.025,0.785398163397448);
#195=CONICAL_SURFACE('',#4438,1.025,0.785398163397448);
#196=CONICAL_SURFACE('',#4446,0.625,0.785398163397448);
#197=CONICAL_SURFACE('',#4450,0.635,0.785398163397449);
#198=CONICAL_SURFACE('',#4454,0.41,0.463647609000806);
#199=CONICAL_SURFACE('',#4458,0.36,0.785398163397448);
#200=CONICAL_SURFACE('',#4479,0.734027674973257,1.0471975511966);
#201=CONICAL_SURFACE('',#4481,0.734027674973257,1.0471975511966);
#202=ORIENTED_CLOSED_SHELL('',*,#3874,.F.);
#203=ORIENTED_CLOSED_SHELL('',*,#3877,.F.);
#204=ORIENTED_CLOSED_SHELL('',*,#3881,.F.);
#205=BREP_WITH_VOIDS('Body1',#3875,(#202));
#206=BREP_WITH_VOIDS('Body1',#3876,(#203));
#207=BREP_WITH_VOIDS('Body1',#3880,(#204));
#208=SHAPE_REPRESENTATION_RELATIONSHIP('SRR','None',#6964,#227);
#209=SHAPE_REPRESENTATION_RELATIONSHIP('SRR','None',#6965,#228);
#210=SHAPE_REPRESENTATION_RELATIONSHIP('SRR','None',#6966,#229);
#211=SHAPE_REPRESENTATION_RELATIONSHIP('SRR','None',#6967,#230);
#212=SHAPE_REPRESENTATION_RELATIONSHIP('SRR','None',#6968,#231);
#213=SHAPE_REPRESENTATION_RELATIONSHIP('SRR','None',#6969,#232);
#214=SHAPE_REPRESENTATION_RELATIONSHIP('SRR','None',#6970,#233);
#215=SHAPE_REPRESENTATION_RELATIONSHIP('SRR','None',#6971,#234);
#216=SHAPE_REPRESENTATION_RELATIONSHIP('SRR','None',#6972,#235);
#217=SHAPE_REPRESENTATION_RELATIONSHIP('SRR','None',#6973,#236);
#218=SHAPE_REPRESENTATION_RELATIONSHIP('SRR','None',#6974,#237);
#219=SHAPE_REPRESENTATION_RELATIONSHIP('SRR','None',#6975,#238);
#220=SHAPE_REPRESENTATION_RELATIONSHIP('SRR','None',#6976,#239);
#221=SHAPE_REPRESENTATION_RELATIONSHIP('SRR','None',#6977,#240);
#222=SHAPE_REPRESENTATION_RELATIONSHIP('SRR','None',#6978,#241);
#223=SHAPE_REPRESENTATION_RELATIONSHIP('SRR','None',#6979,#242);
#224=SHAPE_REPRESENTATION_RELATIONSHIP('SRR','None',#6980,#243);
#225=SHAPE_REPRESENTATION_RELATIONSHIP('SRR','None',#6981,#244);
#226=SHAPE_REPRESENTATION_RELATIONSHIP('SRR','None',#6982,#245);
#227=ADVANCED_BREP_SHAPE_REPRESENTATION('',(#265),#6859);
#228=ADVANCED_BREP_SHAPE_REPRESENTATION('',(#266),#6860);
#229=ADVANCED_BREP_SHAPE_REPRESENTATION('',(#267),#6861);
#230=ADVANCED_BREP_SHAPE_REPRESENTATION('',(#268),#6862);
#231=ADVANCED_BREP_SHAPE_REPRESENTATION('',(#269),#6863);
#232=ADVANCED_BREP_SHAPE_REPRESENTATION('',(#270),#6864);
#233=ADVANCED_BREP_SHAPE_REPRESENTATION('',(#271),#6865);
#234=ADVANCED_BREP_SHAPE_REPRESENTATION('',(#272),#6866);
#235=ADVANCED_BREP_SHAPE_REPRESENTATION('',(#273),#6867);
#236=ADVANCED_BREP_SHAPE_REPRESENTATION('',(#274),#6868);
#237=ADVANCED_BREP_SHAPE_REPRESENTATION('',(#275),#6869);
#238=ADVANCED_BREP_SHAPE_REPRESENTATION('',(#276),#6870);
#239=ADVANCED_BREP_SHAPE_REPRESENTATION('',(#205),#6871);
#240=ADVANCED_BREP_SHAPE_REPRESENTATION('',(#206),#6872);
#241=ADVANCED_BREP_SHAPE_REPRESENTATION('',(#277),#6873);
#242=ADVANCED_BREP_SHAPE_REPRESENTATION('',(#278),#6874);
#243=ADVANCED_BREP_SHAPE_REPRESENTATION('',(#207),#6875);
#244=ADVANCED_BREP_SHAPE_REPRESENTATION('',(#279),#6876);
#245=ADVANCED_BREP_SHAPE_REPRESENTATION('',(#280),#6877);
#246=STYLED_ITEM('',(#7108),#265);
#247=STYLED_ITEM('',(#7143),#266);
#248=STYLED_ITEM('',(#7143),#267);
#249=STYLED_ITEM('',(#7122),#268);
#250=STYLED_ITEM('',(#7143),#269);
#251=STYLED_ITEM('',(#7122),#270);
#252=STYLED_ITEM('',(#7143),#271);
#253=STYLED_ITEM('',(#7122),#272);
#254=STYLED_ITEM('',(#7143),#273);
#255=STYLED_ITEM('',(#7122),#274);
#256=STYLED_ITEM('',(#7122),#275);
#257=STYLED_ITEM('',(#7115),#276);
#258=STYLED_ITEM('',(#7136),#205);
#259=STYLED_ITEM('',(#7136),#206);
#260=STYLED_ITEM('',(#7115),#277);
#261=STYLED_ITEM('',(#7115),#278);
#262=STYLED_ITEM('',(#7136),#207);
#263=STYLED_ITEM('',(#7136),#279);
#264=STYLED_ITEM('',(#7136),#280);
#265=MANIFOLD_SOLID_BREP('Body1',#3862);
#266=MANIFOLD_SOLID_BREP('Body1',#3863);
#267=MANIFOLD_SOLID_BREP('Body1',#3864);
#268=MANIFOLD_SOLID_BREP('Body1',#3865);
#269=MANIFOLD_SOLID_BREP('Body1',#3866);
#270=MANIFOLD_SOLID_BREP('Body1',#3867);
#271=MANIFOLD_SOLID_BREP('Body1',#3868);
#272=MANIFOLD_SOLID_BREP('Body1',#3869);
#273=MANIFOLD_SOLID_BREP('Body1',#3870);
#274=MANIFOLD_SOLID_BREP('Body1',#3871);
#275=MANIFOLD_SOLID_BREP('Body1',#3872);
#276=MANIFOLD_SOLID_BREP('Body1',#3873);
#277=MANIFOLD_SOLID_BREP('Body1',#3878);
#278=MANIFOLD_SOLID_BREP('Body1',#3879);
#279=MANIFOLD_SOLID_BREP('Body1',#3882);
#280=MANIFOLD_SOLID_BREP('Body1',#3883);
#281=FACE_BOUND('',#735,.T.);
#282=FACE_BOUND('',#736,.T.);
#283=FACE_BOUND('',#737,.T.);
#284=FACE_BOUND('',#738,.T.);
#285=FACE_BOUND('',#740,.T.);
#286=FACE_BOUND('',#741,.T.);
#287=FACE_BOUND('',#742,.T.);
#288=FACE_BOUND('',#743,.T.);
#289=FACE_BOUND('',#765,.T.);
#290=FACE_BOUND('',#767,.T.);
#291=FACE_BOUND('',#769,.T.);
#292=FACE_BOUND('',#777,.T.);
#293=FACE_BOUND('',#780,.T.);
#294=FACE_BOUND('',#781,.T.);
#295=FACE_BOUND('',#785,.T.);
#296=FACE_BOUND('',#788,.T.);
#297=FACE_BOUND('',#797,.T.);
#298=FACE_BOUND('',#801,.T.);
#299=FACE_BOUND('',#811,.T.);
#300=FACE_BOUND('',#813,.T.);
#301=FACE_BOUND('',#815,.T.);
#302=FACE_BOUND('',#823,.T.);
#303=FACE_BOUND('',#826,.T.);
#304=FACE_BOUND('',#827,.T.);
#305=FACE_BOUND('',#831,.T.);
#306=FACE_BOUND('',#834,.T.);
#307=FACE_BOUND('',#843,.T.);
#308=FACE_BOUND('',#847,.T.);
#309=FACE_BOUND('',#850,.T.);
#310=FACE_BOUND('',#854,.T.);
#311=FACE_BOUND('',#856,.T.);
#312=FACE_BOUND('',#862,.T.);
#313=FACE_BOUND('',#863,.T.);
#314=FACE_BOUND('',#864,.T.);
#315=FACE_BOUND('',#865,.T.);
#316=FACE_BOUND('',#866,.T.);
#317=FACE_BOUND('',#871,.T.);
#318=FACE_BOUND('',#872,.T.);
#319=FACE_BOUND('',#873,.T.);
#320=FACE_BOUND('',#874,.T.);
#321=FACE_BOUND('',#875,.T.);
#322=FACE_BOUND('',#877,.T.);
#323=FACE_BOUND('',#880,.T.);
#324=FACE_BOUND('',#884,.T.);
#325=FACE_BOUND('',#886,.T.);
#326=FACE_BOUND('',#892,.T.);
#327=FACE_BOUND('',#893,.T.);
#328=FACE_BOUND('',#894,.T.);
#329=FACE_BOUND('',#895,.T.);
#330=FACE_BOUND('',#896,.T.);
#331=FACE_BOUND('',#901,.T.);
#332=FACE_BOUND('',#903,.T.);
#333=FACE_BOUND('',#904,.T.);
#334=FACE_BOUND('',#905,.T.);
#335=FACE_BOUND('',#906,.T.);
#336=FACE_BOUND('',#907,.T.);
#337=FACE_BOUND('',#911,.T.);
#338=FACE_BOUND('',#913,.T.);
#339=FACE_BOUND('',#928,.T.);
#340=FACE_BOUND('',#936,.T.);
#341=FACE_BOUND('',#951,.T.);
#342=FACE_BOUND('',#954,.T.);
#343=FACE_BOUND('',#958,.T.);
#344=FACE_BOUND('',#962,.T.);
#345=FACE_BOUND('',#965,.T.);
#346=FACE_BOUND('',#967,.T.);
#347=FACE_BOUND('',#970,.T.);
#348=FACE_BOUND('',#973,.T.);
#349=FACE_BOUND('',#975,.T.);
#350=FACE_BOUND('',#984,.T.);
#351=FACE_BOUND('',#989,.T.);
#352=FACE_BOUND('',#996,.T.);
#353=FACE_BOUND('',#1012,.T.);
#354=FACE_BOUND('',#1014,.T.);
#355=FACE_BOUND('',#1025,.T.);
#356=FACE_BOUND('',#1027,.T.);
#357=PLANE('',#4108);
#358=PLANE('',#4109);
#359=PLANE('',#4110);
#360=PLANE('',#4111);
#361=PLANE('',#4112);
#362=PLANE('',#4113);
#363=PLANE('',#4115);
#364=PLANE('',#4116);
#365=PLANE('',#4117);
#366=PLANE('',#4118);
#367=PLANE('',#4119);
#368=PLANE('',#4120);
#369=PLANE('',#4122);
#370=PLANE('',#4123);
#371=PLANE('',#4124);
#372=PLANE('',#4125);
#373=PLANE('',#4126);
#374=PLANE('',#4127);
#375=PLANE('',#4132);
#376=PLANE('',#4136);
#377=PLANE('',#4146);
#378=PLANE('',#4147);
#379=PLANE('',#4148);
#380=PLANE('',#4149);
#381=PLANE('',#4150);
#382=PLANE('',#4151);
#383=PLANE('',#4152);
#384=PLANE('',#4153);
#385=PLANE('',#4154);
#386=PLANE('',#4155);
#387=PLANE('',#4156);
#388=PLANE('',#4157);
#389=PLANE('',#4158);
#390=PLANE('',#4159);
#391=PLANE('',#4160);
#392=PLANE('',#4162);
#393=PLANE('',#4167);
#394=PLANE('',#4172);
#395=PLANE('',#4173);
#396=PLANE('',#4181);
#397=PLANE('',#4182);
#398=PLANE('',#4183);
#399=PLANE('',#4184);
#400=PLANE('',#4185);
#401=PLANE('',#4190);
#402=PLANE('',#4194);
#403=PLANE('',#4204);
#404=PLANE('',#4205);
#405=PLANE('',#4206);
#406=PLANE('',#4207);
#407=PLANE('',#4208);
#408=PLANE('',#4209);
#409=PLANE('',#4210);
#410=PLANE('',#4211);
#411=PLANE('',#4212);
#412=PLANE('',#4213);
#413=PLANE('',#4214);
#414=PLANE('',#4215);
#415=PLANE('',#4216);
#416=PLANE('',#4217);
#417=PLANE('',#4218);
#418=PLANE('',#4220);
#419=PLANE('',#4225);
#420=PLANE('',#4230);
#421=PLANE('',#4231);
#422=PLANE('',#4239);
#423=PLANE('',#4240);
#424=PLANE('',#4241);
#425=PLANE('',#4242);
#426=PLANE('',#4243);
#427=PLANE('',#4248);
#428=PLANE('',#4255);
#429=PLANE('',#4256);
#430=PLANE('',#4270);
#431=PLANE('',#4280);
#432=PLANE('',#4281);
#433=PLANE('',#4286);
#434=PLANE('',#4293);
#435=PLANE('',#4294);
#436=PLANE('',#4308);
#437=PLANE('',#4318);
#438=PLANE('',#4319);
#439=PLANE('',#4327);
#440=PLANE('',#4328);
#441=PLANE('',#4330);
#442=PLANE('',#4331);
#443=PLANE('',#4332);
#444=PLANE('',#4333);
#445=PLANE('',#4334);
#446=PLANE('',#4335);
#447=PLANE('',#4336);
#448=PLANE('',#4337);
#449=PLANE('',#4338);
#450=PLANE('',#4340);
#451=PLANE('',#4348);
#452=PLANE('',#4354);
#453=PLANE('',#4362);
#454=PLANE('',#4370);
#455=PLANE('',#4371);
#456=PLANE('',#4372);
#457=PLANE('',#4373);
#458=PLANE('',#4374);
#459=PLANE('',#4375);
#460=PLANE('',#4376);
#461=PLANE('',#4377);
#462=PLANE('',#4378);
#463=PLANE('',#4391);
#464=PLANE('',#4398);
#465=PLANE('',#4407);
#466=PLANE('',#4411);
#467=PLANE('',#4412);
#468=PLANE('',#4417);
#469=PLANE('',#4420);
#470=PLANE('',#4422);
#471=PLANE('',#4424);
#472=PLANE('',#4425);
#473=PLANE('',#4426);
#474=PLANE('',#4427);
#475=PLANE('',#4428);
#476=PLANE('',#4429);
#477=PLANE('',#4432);
#478=PLANE('',#4440);
#479=PLANE('',#4444);
#480=PLANE('',#4452);
#481=PLANE('',#4460);
#482=PLANE('',#4461);
#483=PLANE('',#4462);
#484=PLANE('',#4463);
#485=PLANE('',#4464);
#486=PLANE('',#4465);
#487=PLANE('',#4466);
#488=PLANE('',#4467);
#489=PLANE('',#4468);
#490=PLANE('',#4476);
#491=PLANE('',#4477);
#492=PLANE('',#4483);
#493=PLANE('',#4484);
#494=PLANE('',#4485);
#495=PLANE('',#4489);
#496=PLANE('',#4490);
#497=PLANE('',#4491);
#498=PLANE('',#4492);
#499=PLANE('',#4493);
#500=FACE_OUTER_BOUND('',#726,.T.);
#501=FACE_OUTER_BOUND('',#727,.T.);
#502=FACE_OUTER_BOUND('',#728,.T.);
#503=FACE_OUTER_BOUND('',#729,.T.);
#504=FACE_OUTER_BOUND('',#730,.T.);
#505=FACE_OUTER_BOUND('',#731,.T.);
#506=FACE_OUTER_BOUND('',#732,.T.);
#507=FACE_OUTER_BOUND('',#733,.T.);
#508=FACE_OUTER_BOUND('',#734,.T.);
#509=FACE_OUTER_BOUND('',#739,.T.);
#510=FACE_OUTER_BOUND('',#744,.T.);
#511=FACE_OUTER_BOUND('',#745,.T.);
#512=FACE_OUTER_BOUND('',#746,.T.);
#513=FACE_OUTER_BOUND('',#747,.T.);
#514=FACE_OUTER_BOUND('',#748,.T.);
#515=FACE_OUTER_BOUND('',#749,.T.);
#516=FACE_OUTER_BOUND('',#750,.T.);
#517=FACE_OUTER_BOUND('',#751,.T.);
#518=FACE_OUTER_BOUND('',#752,.T.);
#519=FACE_OUTER_BOUND('',#753,.T.);
#520=FACE_OUTER_BOUND('',#754,.T.);
#521=FACE_OUTER_BOUND('',#755,.T.);
#522=FACE_OUTER_BOUND('',#756,.T.);
#523=FACE_OUTER_BOUND('',#757,.T.);
#524=FACE_OUTER_BOUND('',#758,.T.);
#525=FACE_OUTER_BOUND('',#759,.T.);
#526=FACE_OUTER_BOUND('',#760,.T.);
#527=FACE_OUTER_BOUND('',#761,.T.);
#528=FACE_OUTER_BOUND('',#762,.T.);
#529=FACE_OUTER_BOUND('',#763,.T.);
#530=FACE_OUTER_BOUND('',#764,.T.);
#531=FACE_OUTER_BOUND('',#766,.T.);
#532=FACE_OUTER_BOUND('',#768,.T.);
#533=FACE_OUTER_BOUND('',#770,.T.);
#534=FACE_OUTER_BOUND('',#771,.T.);
#535=FACE_OUTER_BOUND('',#772,.T.);
#536=FACE_OUTER_BOUND('',#773,.T.);
#537=FACE_OUTER_BOUND('',#774,.T.);
#538=FACE_OUTER_BOUND('',#775,.T.);
#539=FACE_OUTER_BOUND('',#776,.T.);
#540=FACE_OUTER_BOUND('',#778,.T.);
#541=FACE_OUTER_BOUND('',#779,.T.);
#542=FACE_OUTER_BOUND('',#782,.T.);
#543=FACE_OUTER_BOUND('',#783,.T.);
#544=FACE_OUTER_BOUND('',#784,.T.);
#545=FACE_OUTER_BOUND('',#786,.T.);
#546=FACE_OUTER_BOUND('',#787,.T.);
#547=FACE_OUTER_BOUND('',#789,.T.);
#548=FACE_OUTER_BOUND('',#790,.T.);
#549=FACE_OUTER_BOUND('',#791,.T.);
#550=FACE_OUTER_BOUND('',#792,.T.);
#551=FACE_OUTER_BOUND('',#793,.T.);
#552=FACE_OUTER_BOUND('',#794,.T.);
#553=FACE_OUTER_BOUND('',#795,.T.);
#554=FACE_OUTER_BOUND('',#796,.T.);
#555=FACE_OUTER_BOUND('',#798,.T.);
#556=FACE_OUTER_BOUND('',#799,.T.);
#557=FACE_OUTER_BOUND('',#800,.T.);
#558=FACE_OUTER_BOUND('',#802,.T.);
#559=FACE_OUTER_BOUND('',#803,.T.);
#560=FACE_OUTER_BOUND('',#804,.T.);
#561=FACE_OUTER_BOUND('',#805,.T.);
#562=FACE_OUTER_BOUND('',#806,.T.);
#563=FACE_OUTER_BOUND('',#807,.T.);
#564=FACE_OUTER_BOUND('',#808,.T.);
#565=FACE_OUTER_BOUND('',#809,.T.);
#566=FACE_OUTER_BOUND('',#810,.T.);
#567=FACE_OUTER_BOUND('',#812,.T.);
#568=FACE_OUTER_BOUND('',#814,.T.);
#569=FACE_OUTER_BOUND('',#816,.T.);
#570=FACE_OUTER_BOUND('',#817,.T.);
#571=FACE_OUTER_BOUND('',#818,.T.);
#572=FACE_OUTER_BOUND('',#819,.T.);
#573=FACE_OUTER_BOUND('',#820,.T.);
#574=FACE_OUTER_BOUND('',#821,.T.);
#575=FACE_OUTER_BOUND('',#822,.T.);
#576=FACE_OUTER_BOUND('',#824,.T.);
#577=FACE_OUTER_BOUND('',#825,.T.);
#578=FACE_OUTER_BOUND('',#828,.T.);
#579=FACE_OUTER_BOUND('',#829,.T.);
#580=FACE_OUTER_BOUND('',#830,.T.);
#581=FACE_OUTER_BOUND('',#832,.T.);
#582=FACE_OUTER_BOUND('',#833,.T.);
#583=FACE_OUTER_BOUND('',#835,.T.);
#584=FACE_OUTER_BOUND('',#836,.T.);
#585=FACE_OUTER_BOUND('',#837,.T.);
#586=FACE_OUTER_BOUND('',#838,.T.);
#587=FACE_OUTER_BOUND('',#839,.T.);
#588=FACE_OUTER_BOUND('',#840,.T.);
#589=FACE_OUTER_BOUND('',#841,.T.);
#590=FACE_OUTER_BOUND('',#842,.T.);
#591=FACE_OUTER_BOUND('',#844,.T.);
#592=FACE_OUTER_BOUND('',#845,.T.);
#593=FACE_OUTER_BOUND('',#846,.T.);
#594=FACE_OUTER_BOUND('',#848,.T.);
#595=FACE_OUTER_BOUND('',#849,.T.);
#596=FACE_OUTER_BOUND('',#851,.T.);
#597=FACE_OUTER_BOUND('',#852,.T.);
#598=FACE_OUTER_BOUND('',#853,.T.);
#599=FACE_OUTER_BOUND('',#855,.T.);
#600=FACE_OUTER_BOUND('',#857,.T.);
#601=FACE_OUTER_BOUND('',#858,.T.);
#602=FACE_OUTER_BOUND('',#859,.T.);
#603=FACE_OUTER_BOUND('',#860,.T.);
#604=FACE_OUTER_BOUND('',#861,.T.);
#605=FACE_OUTER_BOUND('',#867,.T.);
#606=FACE_OUTER_BOUND('',#868,.T.);
#607=FACE_OUTER_BOUND('',#869,.T.);
#608=FACE_OUTER_BOUND('',#870,.T.);
#609=FACE_OUTER_BOUND('',#876,.T.);
#610=FACE_OUTER_BOUND('',#878,.T.);
#611=FACE_OUTER_BOUND('',#879,.T.);
#612=FACE_OUTER_BOUND('',#881,.T.);
#613=FACE_OUTER_BOUND('',#882,.T.);
#614=FACE_OUTER_BOUND('',#883,.T.);
#615=FACE_OUTER_BOUND('',#885,.T.);
#616=FACE_OUTER_BOUND('',#887,.T.);
#617=FACE_OUTER_BOUND('',#888,.T.);
#618=FACE_OUTER_BOUND('',#889,.T.);
#619=FACE_OUTER_BOUND('',#890,.T.);
#620=FACE_OUTER_BOUND('',#891,.T.);
#621=FACE_OUTER_BOUND('',#897,.T.);
#622=FACE_OUTER_BOUND('',#898,.T.);
#623=FACE_OUTER_BOUND('',#899,.T.);
#624=FACE_OUTER_BOUND('',#900,.T.);
#625=FACE_OUTER_BOUND('',#902,.T.);
#626=FACE_OUTER_BOUND('',#908,.T.);
#627=FACE_OUTER_BOUND('',#909,.T.);
#628=FACE_OUTER_BOUND('',#910,.T.);
#629=FACE_OUTER_BOUND('',#912,.T.);
#630=FACE_OUTER_BOUND('',#914,.T.);
#631=FACE_OUTER_BOUND('',#915,.T.);
#632=FACE_OUTER_BOUND('',#916,.T.);
#633=FACE_OUTER_BOUND('',#917,.T.);
#634=FACE_OUTER_BOUND('',#918,.T.);
#635=FACE_OUTER_BOUND('',#919,.T.);
#636=FACE_OUTER_BOUND('',#920,.T.);
#637=FACE_OUTER_BOUND('',#921,.T.);
#638=FACE_OUTER_BOUND('',#922,.T.);
#639=FACE_OUTER_BOUND('',#923,.T.);
#640=FACE_OUTER_BOUND('',#924,.T.);
#641=FACE_OUTER_BOUND('',#925,.T.);
#642=FACE_OUTER_BOUND('',#926,.T.);
#643=FACE_OUTER_BOUND('',#927,.T.);
#644=FACE_OUTER_BOUND('',#929,.T.);
#645=FACE_OUTER_BOUND('',#930,.T.);
#646=FACE_OUTER_BOUND('',#931,.T.);
#647=FACE_OUTER_BOUND('',#932,.T.);
#648=FACE_OUTER_BOUND('',#933,.T.);
#649=FACE_OUTER_BOUND('',#934,.T.);
#650=FACE_OUTER_BOUND('',#935,.T.);
#651=FACE_OUTER_BOUND('',#937,.T.);
#652=FACE_OUTER_BOUND('',#938,.T.);
#653=FACE_OUTER_BOUND('',#939,.T.);
#654=FACE_OUTER_BOUND('',#940,.T.);
#655=FACE_OUTER_BOUND('',#941,.T.);
#656=FACE_OUTER_BOUND('',#942,.T.);
#657=FACE_OUTER_BOUND('',#943,.T.);
#658=FACE_OUTER_BOUND('',#944,.T.);
#659=FACE_OUTER_BOUND('',#945,.T.);
#660=FACE_OUTER_BOUND('',#946,.T.);
#661=FACE_OUTER_BOUND('',#947,.T.);
#662=FACE_OUTER_BOUND('',#948,.T.);
#663=FACE_OUTER_BOUND('',#949,.T.);
#664=FACE_OUTER_BOUND('',#950,.T.);
#665=FACE_OUTER_BOUND('',#952,.T.);
#666=FACE_OUTER_BOUND('',#953,.T.);
#667=FACE_OUTER_BOUND('',#955,.T.);
#668=FACE_OUTER_BOUND('',#956,.T.);
#669=FACE_OUTER_BOUND('',#957,.T.);
#670=FACE_OUTER_BOUND('',#959,.T.);
#671=FACE_OUTER_BOUND('',#960,.T.);
#672=FACE_OUTER_BOUND('',#961,.T.);
#673=FACE_OUTER_BOUND('',#963,.T.);
#674=FACE_OUTER_BOUND('',#964,.T.);
#675=FACE_OUTER_BOUND('',#966,.T.);
#676=FACE_OUTER_BOUND('',#968,.T.);
#677=FACE_OUTER_BOUND('',#969,.T.);
#678=FACE_OUTER_BOUND('',#971,.T.);
#679=FACE_OUTER_BOUND('',#972,.T.);
#680=FACE_OUTER_BOUND('',#974,.T.);
#681=FACE_OUTER_BOUND('',#976,.T.);
#682=FACE_OUTER_BOUND('',#977,.T.);
#683=FACE_OUTER_BOUND('',#978,.T.);
#684=FACE_OUTER_BOUND('',#979,.T.);
#685=FACE_OUTER_BOUND('',#980,.T.);
#686=FACE_OUTER_BOUND('',#981,.T.);
#687=FACE_OUTER_BOUND('',#982,.T.);
#688=FACE_OUTER_BOUND('',#983,.T.);
#689=FACE_OUTER_BOUND('',#985,.T.);
#690=FACE_OUTER_BOUND('',#986,.T.);
#691=FACE_OUTER_BOUND('',#987,.T.);
#692=FACE_OUTER_BOUND('',#988,.T.);
#693=FACE_OUTER_BOUND('',#990,.T.);
#694=FACE_OUTER_BOUND('',#991,.T.);
#695=FACE_OUTER_BOUND('',#992,.T.);
#696=FACE_OUTER_BOUND('',#993,.T.);
#697=FACE_OUTER_BOUND('',#994,.T.);
#698=FACE_OUTER_BOUND('',#995,.T.);
#699=FACE_OUTER_BOUND('',#997,.T.);
#700=FACE_OUTER_BOUND('',#998,.T.);
#701=FACE_OUTER_BOUND('',#999,.T.);
#702=FACE_OUTER_BOUND('',#1000,.T.);
#703=FACE_OUTER_BOUND('',#1001,.T.);
#704=FACE_OUTER_BOUND('',#1002,.T.);
#705=FACE_OUTER_BOUND('',#1003,.T.);
#706=FACE_OUTER_BOUND('',#1004,.T.);
#707=FACE_OUTER_BOUND('',#1005,.T.);
#708=FACE_OUTER_BOUND('',#1006,.T.);
#709=FACE_OUTER_BOUND('',#1007,.T.);
#710=FACE_OUTER_BOUND('',#1008,.T.);
#711=FACE_OUTER_BOUND('',#1009,.T.);
#712=FACE_OUTER_BOUND('',#1010,.T.);
#713=FACE_OUTER_BOUND('',#1011,.T.);
#714=FACE_OUTER_BOUND('',#1013,.T.);
#715=FACE_OUTER_BOUND('',#1015,.T.);
#716=FACE_OUTER_BOUND('',#1016,.T.);
#717=FACE_OUTER_BOUND('',#1017,.T.);
#718=FACE_OUTER_BOUND('',#1018,.T.);
#719=FACE_OUTER_BOUND('',#1019,.T.);
#720=FACE_OUTER_BOUND('',#1020,.T.);
#721=FACE_OUTER_BOUND('',#1021,.T.);
#722=FACE_OUTER_BOUND('',#1022,.T.);
#723=FACE_OUTER_BOUND('',#1023,.T.);
#724=FACE_OUTER_BOUND('',#1024,.T.);
#725=FACE_OUTER_BOUND('',#1026,.T.);
#726=EDGE_LOOP('',(#2608,#2609,#2610,#2611));
#727=EDGE_LOOP('',(#2612,#2613,#2614,#2615));
#728=EDGE_LOOP('',(#2616,#2617,#2618,#2619));
#729=EDGE_LOOP('',(#2620,#2621,#2622,#2623));
#730=EDGE_LOOP('',(#2624,#2625,#2626,#2627));
#731=EDGE_LOOP('',(#2628,#2629,#2630,#2631));
#732=EDGE_LOOP('',(#2632,#2633,#2634,#2635));
#733=EDGE_LOOP('',(#2636,#2637,#2638,#2639));
#734=EDGE_LOOP('',(#2640,#2641,#2642,#2643));
#735=EDGE_LOOP('',(#2644));
#736=EDGE_LOOP('',(#2645));
#737=EDGE_LOOP('',(#2646));
#738=EDGE_LOOP('',(#2647));
#739=EDGE_LOOP('',(#2648,#2649,#2650,#2651));
#740=EDGE_LOOP('',(#2652));
#741=EDGE_LOOP('',(#2653));
#742=EDGE_LOOP('',(#2654));
#743=EDGE_LOOP('',(#2655));
#744=EDGE_LOOP('',(#2656,#2657,#2658,#2659));
#745=EDGE_LOOP('',(#2660,#2661,#2662,#2663));
#746=EDGE_LOOP('',(#2664,#2665,#2666,#2667));
#747=EDGE_LOOP('',(#2668,#2669,#2670,#2671));
#748=EDGE_LOOP('',(#2672,#2673,#2674,#2675));
#749=EDGE_LOOP('',(#2676,#2677,#2678,#2679));
#750=EDGE_LOOP('',(#2680,#2681,#2682,#2683));
#751=EDGE_LOOP('',(#2684,#2685,#2686,#2687));
#752=EDGE_LOOP('',(#2688,#2689,#2690,#2691));
#753=EDGE_LOOP('',(#2692,#2693,#2694,#2695));
#754=EDGE_LOOP('',(#2696,#2697,#2698,#2699));
#755=EDGE_LOOP('',(#2700,#2701,#2702,#2703));
#756=EDGE_LOOP('',(#2704,#2705,#2706,#2707));
#757=EDGE_LOOP('',(#2708));
#758=EDGE_LOOP('',(#2709,#2710,#2711,#2712));
#759=EDGE_LOOP('',(#2713));
#760=EDGE_LOOP('',(#2714,#2715,#2716,#2717));
#761=EDGE_LOOP('',(#2718,#2719,#2720,#2721));
#762=EDGE_LOOP('',(#2722,#2723,#2724,#2725));
#763=EDGE_LOOP('',(#2726,#2727,#2728,#2729,#2730,#2731,#2732,#2733,#2734,
#2735,#2736,#2737,#2738,#2739));
#764=EDGE_LOOP('',(#2740,#2741,#2742,#2743));
#765=EDGE_LOOP('',(#2744));
#766=EDGE_LOOP('',(#2745,#2746,#2747,#2748));
#767=EDGE_LOOP('',(#2749));
#768=EDGE_LOOP('',(#2750,#2751,#2752,#2753));
#769=EDGE_LOOP('',(#2754));
#770=EDGE_LOOP('',(#2755,#2756,#2757,#2758));
#771=EDGE_LOOP('',(#2759,#2760,#2761,#2762));
#772=EDGE_LOOP('',(#2763,#2764,#2765,#2766));
#773=EDGE_LOOP('',(#2767,#2768,#2769,#2770));
#774=EDGE_LOOP('',(#2771,#2772,#2773,#2774));
#775=EDGE_LOOP('',(#2775,#2776,#2777,#2778));
#776=EDGE_LOOP('',(#2779,#2780,#2781,#2782));
#777=EDGE_LOOP('',(#2783));
#778=EDGE_LOOP('',(#2784,#2785,#2786,#2787));
#779=EDGE_LOOP('',(#2788,#2789,#2790,#2791));
#780=EDGE_LOOP('',(#2792));
#781=EDGE_LOOP('',(#2793));
#782=EDGE_LOOP('',(#2794,#2795,#2796,#2797));
#783=EDGE_LOOP('',(#2798,#2799,#2800,#2801,#2802,#2803,#2804,#2805,#2806,
#2807,#2808,#2809,#2810,#2811));
#784=EDGE_LOOP('',(#2812,#2813));
#785=EDGE_LOOP('',(#2814));
#786=EDGE_LOOP('',(#2815,#2816,#2817,#2818));
#787=EDGE_LOOP('',(#2819,#2820));
#788=EDGE_LOOP('',(#2821));
#789=EDGE_LOOP('',(#2822,#2823,#2824,#2825));
#790=EDGE_LOOP('',(#2826,#2827,#2828,#2829,#2830,#2831,#2832,#2833));
#791=EDGE_LOOP('',(#2834,#2835,#2836,#2837,#2838,#2839,#2840,#2841));
#792=EDGE_LOOP('',(#2842,#2843,#2844,#2845));
#793=EDGE_LOOP('',(#2846,#2847,#2848,#2849));
#794=EDGE_LOOP('',(#2850,#2851,#2852,#2853));
#795=EDGE_LOOP('',(#2854,#2855,#2856,#2857,#2858,#2859));
#796=EDGE_LOOP('',(#2860,#2861,#2862,#2863));
#797=EDGE_LOOP('',(#2864));
#798=EDGE_LOOP('',(#2865,#2866,#2867,#2868,#2869,#2870));
#799=EDGE_LOOP('',(#2871,#2872,#2873,#2874,#2875,#2876,#2877,#2878));
#800=EDGE_LOOP('',(#2879,#2880,#2881,#2882));
#801=EDGE_LOOP('',(#2883));
#802=EDGE_LOOP('',(#2884,#2885,#2886,#2887));
#803=EDGE_LOOP('',(#2888));
#804=EDGE_LOOP('',(#2889,#2890,#2891,#2892));
#805=EDGE_LOOP('',(#2893));
#806=EDGE_LOOP('',(#2894,#2895,#2896,#2897));
#807=EDGE_LOOP('',(#2898,#2899,#2900,#2901));
#808=EDGE_LOOP('',(#2902,#2903,#2904,#2905));
#809=EDGE_LOOP('',(#2906,#2907,#2908,#2909,#2910,#2911,#2912,#2913,#2914,
#2915,#2916,#2917,#2918,#2919));
#810=EDGE_LOOP('',(#2920,#2921,#2922,#2923));
#811=EDGE_LOOP('',(#2924));
#812=EDGE_LOOP('',(#2925,#2926,#2927,#2928));
#813=EDGE_LOOP('',(#2929));
#814=EDGE_LOOP('',(#2930,#2931,#2932,#2933));
#815=EDGE_LOOP('',(#2934));
#816=EDGE_LOOP('',(#2935,#2936,#2937,#2938));
#817=EDGE_LOOP('',(#2939,#2940,#2941,#2942));
#818=EDGE_LOOP('',(#2943,#2944,#2945,#2946));
#819=EDGE_LOOP('',(#2947,#2948,#2949,#2950));
#820=EDGE_LOOP('',(#2951,#2952,#2953,#2954));
#821=EDGE_LOOP('',(#2955,#2956,#2957,#2958));
#822=EDGE_LOOP('',(#2959,#2960,#2961,#2962));
#823=EDGE_LOOP('',(#2963));
#824=EDGE_LOOP('',(#2964,#2965,#2966,#2967));
#825=EDGE_LOOP('',(#2968,#2969,#2970,#2971));
#826=EDGE_LOOP('',(#2972));
#827=EDGE_LOOP('',(#2973));
#828=EDGE_LOOP('',(#2974,#2975,#2976,#2977));
#829=EDGE_LOOP('',(#2978,#2979,#2980,#2981,#2982,#2983,#2984,#2985,#2986,
#2987,#2988,#2989,#2990,#2991));
#830=EDGE_LOOP('',(#2992,#2993));
#831=EDGE_LOOP('',(#2994));
#832=EDGE_LOOP('',(#2995,#2996,#2997,#2998));
#833=EDGE_LOOP('',(#2999,#3000));
#834=EDGE_LOOP('',(#3001));
#835=EDGE_LOOP('',(#3002,#3003,#3004,#3005));
#836=EDGE_LOOP('',(#3006,#3007,#3008,#3009,#3010,#3011,#3012,#3013));
#837=EDGE_LOOP('',(#3014,#3015,#3016,#3017,#3018,#3019,#3020,#3021));
#838=EDGE_LOOP('',(#3022,#3023,#3024,#3025));
#839=EDGE_LOOP('',(#3026,#3027,#3028,#3029));
#840=EDGE_LOOP('',(#3030,#3031,#3032,#3033));
#841=EDGE_LOOP('',(#3034,#3035,#3036,#3037,#3038,#3039));
#842=EDGE_LOOP('',(#3040,#3041,#3042,#3043));
#843=EDGE_LOOP('',(#3044));
#844=EDGE_LOOP('',(#3045,#3046,#3047,#3048,#3049,#3050));
#845=EDGE_LOOP('',(#3051,#3052,#3053,#3054,#3055,#3056,#3057,#3058));
#846=EDGE_LOOP('',(#3059,#3060,#3061,#3062));
#847=EDGE_LOOP('',(#3063));
#848=EDGE_LOOP('',(#3064,#3065,#3066,#3067));
#849=EDGE_LOOP('',(#3068));
#850=EDGE_LOOP('',(#3069));
#851=EDGE_LOOP('',(#3070,#3071,#3072,#3073));
#852=EDGE_LOOP('',(#3074,#3075,#3076,#3077));
#853=EDGE_LOOP('',(#3078));
#854=EDGE_LOOP('',(#3079));
#855=EDGE_LOOP('',(#3080));
#856=EDGE_LOOP('',(#3081));
#857=EDGE_LOOP('',(#3082,#3083,#3084,#3085));
#858=EDGE_LOOP('',(#3086,#3087,#3088,#3089));
#859=EDGE_LOOP('',(#3090,#3091,#3092,#3093));
#860=EDGE_LOOP('',(#3094,#3095,#3096,#3097));
#861=EDGE_LOOP('',(#3098));
#862=EDGE_LOOP('',(#3099));
#863=EDGE_LOOP('',(#3100));
#864=EDGE_LOOP('',(#3101));
#865=EDGE_LOOP('',(#3102));
#866=EDGE_LOOP('',(#3103));
#867=EDGE_LOOP('',(#3104,#3105,#3106,#3107));
#868=EDGE_LOOP('',(#3108,#3109,#3110,#3111));
#869=EDGE_LOOP('',(#3112,#3113,#3114,#3115));
#870=EDGE_LOOP('',(#3116));
#871=EDGE_LOOP('',(#3117));
#872=EDGE_LOOP('',(#3118));
#873=EDGE_LOOP('',(#3119));
#874=EDGE_LOOP('',(#3120));
#875=EDGE_LOOP('',(#3121));
#876=EDGE_LOOP('',(#3122));
#877=EDGE_LOOP('',(#3123));
#878=EDGE_LOOP('',(#3124,#3125,#3126,#3127));
#879=EDGE_LOOP('',(#3128));
#880=EDGE_LOOP('',(#3129));
#881=EDGE_LOOP('',(#3130,#3131,#3132,#3133));
#882=EDGE_LOOP('',(#3134,#3135,#3136,#3137));
#883=EDGE_LOOP('',(#3138));
#884=EDGE_LOOP('',(#3139));
#885=EDGE_LOOP('',(#3140));
#886=EDGE_LOOP('',(#3141));
#887=EDGE_LOOP('',(#3142,#3143,#3144,#3145));
#888=EDGE_LOOP('',(#3146,#3147,#3148,#3149));
#889=EDGE_LOOP('',(#3150,#3151,#3152,#3153));
#890=EDGE_LOOP('',(#3154,#3155,#3156,#3157));
#891=EDGE_LOOP('',(#3158));
#892=EDGE_LOOP('',(#3159));
#893=EDGE_LOOP('',(#3160));
#894=EDGE_LOOP('',(#3161));
#895=EDGE_LOOP('',(#3162));
#896=EDGE_LOOP('',(#3163));
#897=EDGE_LOOP('',(#3164,#3165,#3166,#3167));
#898=EDGE_LOOP('',(#3168,#3169,#3170,#3171));
#899=EDGE_LOOP('',(#3172,#3173,#3174,#3175));
#900=EDGE_LOOP('',(#3176));
#901=EDGE_LOOP('',(#3177));
#902=EDGE_LOOP('',(#3178));
#903=EDGE_LOOP('',(#3179));
#904=EDGE_LOOP('',(#3180));
#905=EDGE_LOOP('',(#3181));
#906=EDGE_LOOP('',(#3182));
#907=EDGE_LOOP('',(#3183));
#908=EDGE_LOOP('',(#3184,#3185,#3186,#3187));
#909=EDGE_LOOP('',(#3188,#3189,#3190,#3191));
#910=EDGE_LOOP('',(#3192));
#911=EDGE_LOOP('',(#3193));
#912=EDGE_LOOP('',(#3194));
#913=EDGE_LOOP('',(#3195));
#914=EDGE_LOOP('',(#3196,#3197,#3198,#3199));
#915=EDGE_LOOP('',(#3200,#3201,#3202,#3203));
#916=EDGE_LOOP('',(#3204,#3205,#3206,#3207));
#917=EDGE_LOOP('',(#3208,#3209,#3210,#3211));
#918=EDGE_LOOP('',(#3212,#3213,#3214,#3215));
#919=EDGE_LOOP('',(#3216,#3217,#3218,#3219));
#920=EDGE_LOOP('',(#3220,#3221,#3222,#3223,#3224,#3225));
#921=EDGE_LOOP('',(#3226,#3227,#3228,#3229,#3230,#3231));
#922=EDGE_LOOP('',(#3232));
#923=EDGE_LOOP('',(#3233));
#924=EDGE_LOOP('',(#3234,#3235,#3236,#3237));
#925=EDGE_LOOP('',(#3238,#3239,#3240,#3241));
#926=EDGE_LOOP('',(#3242,#3243,#3244,#3245));
#927=EDGE_LOOP('',(#3246));
#928=EDGE_LOOP('',(#3247));
#929=EDGE_LOOP('',(#3248,#3249,#3250,#3251));
#930=EDGE_LOOP('',(#3252,#3253,#3254,#3255));
#931=EDGE_LOOP('',(#3256));
#932=EDGE_LOOP('',(#3257,#3258,#3259,#3260));
#933=EDGE_LOOP('',(#3261,#3262,#3263,#3264));
#934=EDGE_LOOP('',(#3265,#3266,#3267,#3268));
#935=EDGE_LOOP('',(#3269));
#936=EDGE_LOOP('',(#3270));
#937=EDGE_LOOP('',(#3271,#3272,#3273,#3274));
#938=EDGE_LOOP('',(#3275,#3276,#3277,#3278));
#939=EDGE_LOOP('',(#3279,#3280,#3281,#3282));
#940=EDGE_LOOP('',(#3283));
#941=EDGE_LOOP('',(#3284,#3285,#3286,#3287));
#942=EDGE_LOOP('',(#3288,#3289,#3290,#3291));
#943=EDGE_LOOP('',(#3292,#3293,#3294,#3295));
#944=EDGE_LOOP('',(#3296,#3297,#3298,#3299));
#945=EDGE_LOOP('',(#3300,#3301,#3302,#3303));
#946=EDGE_LOOP('',(#3304,#3305,#3306,#3307));
#947=EDGE_LOOP('',(#3308,#3309,#3310,#3311,#3312,#3313));
#948=EDGE_LOOP('',(#3314,#3315,#3316,#3317,#3318,#3319));
#949=EDGE_LOOP('',(#3320,#3321,#3322,#3323,#3324,#3325));
#950=EDGE_LOOP('',(#3326,#3327));
#951=EDGE_LOOP('',(#3328,#3329,#3330,#3331));
#952=EDGE_LOOP('',(#3332,#3333,#3334,#3335,#3336,#3337));
#953=EDGE_LOOP('',(#3338));
#954=EDGE_LOOP('',(#3339));
#955=EDGE_LOOP('',(#3340,#3341,#3342,#3343));
#956=EDGE_LOOP('',(#3344,#3345,#3346,#3347));
#957=EDGE_LOOP('',(#3348));
#958=EDGE_LOOP('',(#3349));
#959=EDGE_LOOP('',(#3350,#3351,#3352,#3353));
#960=EDGE_LOOP('',(#3354,#3355,#3356,#3357,#3358,#3359));
#961=EDGE_LOOP('',(#3360));
#962=EDGE_LOOP('',(#3361));
#963=EDGE_LOOP('',(#3362,#3363,#3364,#3365));
#964=EDGE_LOOP('',(#3366));
#965=EDGE_LOOP('',(#3367));
#966=EDGE_LOOP('',(#3368));
#967=EDGE_LOOP('',(#3369));
#968=EDGE_LOOP('',(#3370,#3371,#3372,#3373));
#969=EDGE_LOOP('',(#3374));
#970=EDGE_LOOP('',(#3375));
#971=EDGE_LOOP('',(#3376,#3377,#3378,#3379,#3380,#3381));
#972=EDGE_LOOP('',(#3382,#3383,#3384,#3385,#3386,#3387));
#973=EDGE_LOOP('',(#3388));
#974=EDGE_LOOP('',(#3389,#3390,#3391,#3392,#3393,#3394));
#975=EDGE_LOOP('',(#3395));
#976=EDGE_LOOP('',(#3396,#3397,#3398,#3399));
#977=EDGE_LOOP('',(#3400,#3401,#3402,#3403));
#978=EDGE_LOOP('',(#3404,#3405,#3406,#3407));
#979=EDGE_LOOP('',(#3408,#3409,#3410,#3411));
#980=EDGE_LOOP('',(#3412,#3413,#3414,#3415));
#981=EDGE_LOOP('',(#3416,#3417,#3418,#3419));
#982=EDGE_LOOP('',(#3420,#3421,#3422,#3423));
#983=EDGE_LOOP('',(#3424));
#984=EDGE_LOOP('',(#3425));
#985=EDGE_LOOP('',(#3426,#3427,#3428,#3429));
#986=EDGE_LOOP('',(#3430,#3431,#3432,#3433));
#987=EDGE_LOOP('',(#3434,#3435,#3436,#3437));
#988=EDGE_LOOP('',(#3438));
#989=EDGE_LOOP('',(#3439));
#990=EDGE_LOOP('',(#3440,#3441,#3442,#3443));
#991=EDGE_LOOP('',(#3444));
#992=EDGE_LOOP('',(#3445,#3446,#3447,#3448));
#993=EDGE_LOOP('',(#3449,#3450,#3451,#3452));
#994=EDGE_LOOP('',(#3453,#3454,#3455,#3456));
#995=EDGE_LOOP('',(#3457));
#996=EDGE_LOOP('',(#3458));
#997=EDGE_LOOP('',(#3459,#3460,#3461,#3462));
#998=EDGE_LOOP('',(#3463,#3464,#3465,#3466));
#999=EDGE_LOOP('',(#3467,#3468,#3469,#3470));
#1000=EDGE_LOOP('',(#3471));
#1001=EDGE_LOOP('',(#3472,#3473,#3474,#3475));
#1002=EDGE_LOOP('',(#3476,#3477,#3478,#3479));
#1003=EDGE_LOOP('',(#3480,#3481,#3482,#3483));
#1004=EDGE_LOOP('',(#3484,#3485,#3486,#3487));
#1005=EDGE_LOOP('',(#3488,#3489,#3490,#3491));
#1006=EDGE_LOOP('',(#3492,#3493,#3494,#3495));
#1007=EDGE_LOOP('',(#3496,#3497,#3498,#3499,#3500,#3501));
#1008=EDGE_LOOP('',(#3502,#3503,#3504,#3505,#3506,#3507));
#1009=EDGE_LOOP('',(#3508,#3509,#3510,#3511));
#1010=EDGE_LOOP('',(#3512,#3513,#3514,#3515));
#1011=EDGE_LOOP('',(#3516));
#1012=EDGE_LOOP('',(#3517));
#1013=EDGE_LOOP('',(#3518));
#1014=EDGE_LOOP('',(#3519));
#1015=EDGE_LOOP('',(#3520,#3521,#3522,#3523,#3524,#3525,#3526,#3527,#3528));
#1016=EDGE_LOOP('',(#3529,#3530,#3531,#3532,#3533,#3534,#3535,#3536,#3537));
#1017=EDGE_LOOP('',(#3538,#3539,#3540,#3541));
#1018=EDGE_LOOP('',(#3542,#3543,#3544,#3545));
#1019=EDGE_LOOP('',(#3546,#3547,#3548,#3549));
#1020=EDGE_LOOP('',(#3550,#3551,#3552,#3553));
#1021=EDGE_LOOP('',(#3554,#3555,#3556,#3557));
#1022=EDGE_LOOP('',(#3558,#3559,#3560,#3561));
#1023=EDGE_LOOP('',(#3562,#3563,#3564,#3565));
#1024=EDGE_LOOP('',(#3566));
#1025=EDGE_LOOP('',(#3567));
#1026=EDGE_LOOP('',(#3568));
#1027=EDGE_LOOP('',(#3569));
#1028=LINE('',#5735,#1343);
#1029=LINE('',#5741,#1344);
#1030=LINE('',#5747,#1345);
#1031=LINE('',#5753,#1346);
#1032=LINE('',#5758,#1347);
#1033=LINE('',#5760,#1348);
#1034=LINE('',#5762,#1349);
#1035=LINE('',#5763,#1350);
#1036=LINE('',#5766,#1351);
#1037=LINE('',#5768,#1352);
#1038=LINE('',#5769,#1353);
#1039=LINE('',#5772,#1354);
#1040=LINE('',#5774,#1355);
#1041=LINE('',#5775,#1356);
#1042=LINE('',#5777,#1357);
#1043=LINE('',#5778,#1358);
#1044=LINE('',#5785,#1359);
#1045=LINE('',#5787,#1360);
#1046=LINE('',#5789,#1361);
#1047=LINE('',#5790,#1362);
#1048=LINE('',#5793,#1363);
#1049=LINE('',#5795,#1364);
#1050=LINE('',#5796,#1365);
#1051=LINE('',#5799,#1366);
#1052=LINE('',#5801,#1367);
#1053=LINE('',#5802,#1368);
#1054=LINE('',#5804,#1369);
#1055=LINE('',#5805,#1370);
#1056=LINE('',#5812,#1371);
#1057=LINE('',#5814,#1372);
#1058=LINE('',#5816,#1373);
#1059=LINE('',#5817,#1374);
#1060=LINE('',#5820,#1375);
#1061=LINE('',#5822,#1376);
#1062=LINE('',#5823,#1377);
#1063=LINE('',#5826,#1378);
#1064=LINE('',#5828,#1379);
#1065=LINE('',#5829,#1380);
#1066=LINE('',#5831,#1381);
#1067=LINE('',#5832,#1382);
#1068=LINE('',#5840,#1383);
#1069=LINE('',#5847,#1384);
#1070=LINE('',#5854,#1385);
#1071=LINE('',#5860,#1386);
#1072=LINE('',#5865,#1387);
#1073=LINE('',#5869,#1388);
#1074=LINE('',#5873,#1389);
#1075=LINE('',#5875,#1390);
#1076=LINE('',#5877,#1391);
#1077=LINE('',#5879,#1392);
#1078=LINE('',#5881,#1393);
#1079=LINE('',#5883,#1394);
#1080=LINE('',#5885,#1395);
#1081=LINE('',#5887,#1396);
#1082=LINE('',#5889,#1397);
#1083=LINE('',#5891,#1398);
#1084=LINE('',#5893,#1399);
#1085=LINE('',#5895,#1400);
#1086=LINE('',#5896,#1401);
#1087=LINE('',#5899,#1402);
#1088=LINE('',#5900,#1403);
#1089=LINE('',#5903,#1404);
#1090=LINE('',#5904,#1405);
#1091=LINE('',#5908,#1406);
#1092=LINE('',#5909,#1407);
#1093=LINE('',#5910,#1408);
#1094=LINE('',#5913,#1409);
#1095=LINE('',#5914,#1410);
#1096=LINE('',#5917,#1411);
#1097=LINE('',#5918,#1412);
#1098=LINE('',#5920,#1413);
#1099=LINE('',#5923,#1414);
#1100=LINE('',#5924,#1415);
#1101=LINE('',#5927,#1416);
#1102=LINE('',#5928,#1417);
#1103=LINE('',#5931,#1418);
#1104=LINE('',#5932,#1419);
#1105=LINE('',#5935,#1420);
#1106=LINE('',#5936,#1421);
#1107=LINE('',#5939,#1422);
#1108=LINE('',#5940,#1423);
#1109=LINE('',#5943,#1424);
#1110=LINE('',#5944,#1425);
#1111=LINE('',#5946,#1426);
#1112=LINE('',#5952,#1427);
#1113=LINE('',#5958,#1428);
#1114=LINE('',#5961,#1429);
#1115=LINE('',#5965,#1430);
#1116=LINE('',#5971,#1431);
#1117=LINE('',#5974,#1432);
#1118=LINE('',#5977,#1433);
#1119=LINE('',#5979,#1434);
#1120=LINE('',#5981,#1435);
#1121=LINE('',#5983,#1436);
#1122=LINE('',#5984,#1437);
#1123=LINE('',#5987,#1438);
#1124=LINE('',#5989,#1439);
#1125=LINE('',#5991,#1440);
#1126=LINE('',#5993,#1441);
#1127=LINE('',#5994,#1442);
#1128=LINE('',#5998,#1443);
#1129=LINE('',#6002,#1444);
#1130=LINE('',#6008,#1445);
#1131=LINE('',#6011,#1446);
#1132=LINE('',#6013,#1447);
#1133=LINE('',#6014,#1448);
#1134=LINE('',#6015,#1449);
#1135=LINE('',#6017,#1450);
#1136=LINE('',#6019,#1451);
#1137=LINE('',#6020,#1452);
#1138=LINE('',#6028,#1453);
#1139=LINE('',#6035,#1454);
#1140=LINE('',#6042,#1455);
#1141=LINE('',#6048,#1456);
#1142=LINE('',#6053,#1457);
#1143=LINE('',#6057,#1458);
#1144=LINE('',#6061,#1459);
#1145=LINE('',#6063,#1460);
#1146=LINE('',#6065,#1461);
#1147=LINE('',#6067,#1462);
#1148=LINE('',#6069,#1463);
#1149=LINE('',#6071,#1464);
#1150=LINE('',#6073,#1465);
#1151=LINE('',#6075,#1466);
#1152=LINE('',#6077,#1467);
#1153=LINE('',#6079,#1468);
#1154=LINE('',#6081,#1469);
#1155=LINE('',#6083,#1470);
#1156=LINE('',#6084,#1471);
#1157=LINE('',#6087,#1472);
#1158=LINE('',#6088,#1473);
#1159=LINE('',#6091,#1474);
#1160=LINE('',#6092,#1475);
#1161=LINE('',#6096,#1476);
#1162=LINE('',#6097,#1477);
#1163=LINE('',#6098,#1478);
#1164=LINE('',#6101,#1479);
#1165=LINE('',#6102,#1480);
#1166=LINE('',#6105,#1481);
#1167=LINE('',#6106,#1482);
#1168=LINE('',#6108,#1483);
#1169=LINE('',#6111,#1484);
#1170=LINE('',#6112,#1485);
#1171=LINE('',#6115,#1486);
#1172=LINE('',#6116,#1487);
#1173=LINE('',#6119,#1488);
#1174=LINE('',#6120,#1489);
#1175=LINE('',#6123,#1490);
#1176=LINE('',#6124,#1491);
#1177=LINE('',#6127,#1492);
#1178=LINE('',#6128,#1493);
#1179=LINE('',#6131,#1494);
#1180=LINE('',#6132,#1495);
#1181=LINE('',#6134,#1496);
#1182=LINE('',#6140,#1497);
#1183=LINE('',#6146,#1498);
#1184=LINE('',#6149,#1499);
#1185=LINE('',#6153,#1500);
#1186=LINE('',#6159,#1501);
#1187=LINE('',#6162,#1502);
#1188=LINE('',#6165,#1503);
#1189=LINE('',#6167,#1504);
#1190=LINE('',#6169,#1505);
#1191=LINE('',#6171,#1506);
#1192=LINE('',#6172,#1507);
#1193=LINE('',#6175,#1508);
#1194=LINE('',#6177,#1509);
#1195=LINE('',#6179,#1510);
#1196=LINE('',#6181,#1511);
#1197=LINE('',#6182,#1512);
#1198=LINE('',#6186,#1513);
#1199=LINE('',#6190,#1514);
#1200=LINE('',#6196,#1515);
#1201=LINE('',#6199,#1516);
#1202=LINE('',#6201,#1517);
#1203=LINE('',#6202,#1518);
#1204=LINE('',#6203,#1519);
#1205=LINE('',#6205,#1520);
#1206=LINE('',#6207,#1521);
#1207=LINE('',#6208,#1522);
#1208=LINE('',#6216,#1523);
#1209=LINE('',#6224,#1524);
#1210=LINE('',#6229,#1525);
#1211=LINE('',#6238,#1526);
#1212=LINE('',#6244,#1527);
#1213=LINE('',#6250,#1528);
#1214=LINE('',#6256,#1529);
#1215=LINE('',#6266,#1530);
#1216=LINE('',#6271,#1531);
#1217=LINE('',#6275,#1532);
#1218=LINE('',#6284,#1533);
#1219=LINE('',#6291,#1534);
#1220=LINE('',#6297,#1535);
#1221=LINE('',#6306,#1536);
#1222=LINE('',#6312,#1537);
#1223=LINE('',#6318,#1538);
#1224=LINE('',#6324,#1539);
#1225=LINE('',#6333,#1540);
#1226=LINE('',#6339,#1541);
#1227=LINE('',#6344,#1542);
#1228=LINE('',#6352,#1543);
#1229=LINE('',#6358,#1544);
#1230=LINE('',#6366,#1545);
#1231=LINE('',#6368,#1546);
#1232=LINE('',#6370,#1547);
#1233=LINE('',#6371,#1548);
#1234=LINE('',#6374,#1549);
#1235=LINE('',#6376,#1550);
#1236=LINE('',#6377,#1551);
#1237=LINE('',#6380,#1552);
#1238=LINE('',#6382,#1553);
#1239=LINE('',#6383,#1554);
#1240=LINE('',#6386,#1555);
#1241=LINE('',#6388,#1556);
#1242=LINE('',#6389,#1557);
#1243=LINE('',#6392,#1558);
#1244=LINE('',#6394,#1559);
#1245=LINE('',#6395,#1560);
#1246=LINE('',#6397,#1561);
#1247=LINE('',#6398,#1562);
#1248=LINE('',#6410,#1563);
#1249=LINE('',#6414,#1564);
#1250=LINE('',#6418,#1565);
#1251=LINE('',#6425,#1566);
#1252=LINE('',#6427,#1567);
#1253=LINE('',#6435,#1568);
#1254=LINE('',#6439,#1569);
#1255=LINE('',#6443,#1570);
#1256=LINE('',#6450,#1571);
#1257=LINE('',#6454,#1572);
#1258=LINE('',#6458,#1573);
#1259=LINE('',#6463,#1574);
#1260=LINE('',#6465,#1575);
#1261=LINE('',#6467,#1576);
#1262=LINE('',#6468,#1577);
#1263=LINE('',#6471,#1578);
#1264=LINE('',#6473,#1579);
#1265=LINE('',#6474,#1580);
#1266=LINE('',#6477,#1581);
#1267=LINE('',#6479,#1582);
#1268=LINE('',#6480,#1583);
#1269=LINE('',#6483,#1584);
#1270=LINE('',#6485,#1585);
#1271=LINE('',#6486,#1586);
#1272=LINE('',#6489,#1587);
#1273=LINE('',#6491,#1588);
#1274=LINE('',#6492,#1589);
#1275=LINE('',#6494,#1590);
#1276=LINE('',#6495,#1591);
#1277=LINE('',#6506,#1592);
#1278=LINE('',#6518,#1593);
#1279=LINE('',#6526,#1594);
#1280=LINE('',#6531,#1595);
#1281=LINE('',#6546,#1596);
#1282=LINE('',#6554,#1597);
#1283=LINE('',#6564,#1598);
#1284=LINE('',#6567,#1599);
#1285=LINE('',#6572,#1600);
#1286=LINE('',#6574,#1601);
#1287=LINE('',#6576,#1602);
#1288=LINE('',#6578,#1603);
#1289=LINE('',#6580,#1604);
#1290=LINE('',#6581,#1605);
#1291=LINE('',#6587,#1606);
#1292=LINE('',#6589,#1607);
#1293=LINE('',#6591,#1608);
#1294=LINE('',#6593,#1609);
#1295=LINE('',#6595,#1610);
#1296=LINE('',#6596,#1611);
#1297=LINE('',#6600,#1612);
#1298=LINE('',#6601,#1613);
#1299=LINE('',#6603,#1614);
#1300=LINE('',#6605,#1615);
#1301=LINE('',#6607,#1616);
#1302=LINE('',#6609,#1617);
#1303=LINE('',#6613,#1618);
#1304=LINE('',#6621,#1619);
#1305=LINE('',#6625,#1620);
#1306=LINE('',#6629,#1621);
#1307=LINE('',#6634,#1622);
#1308=LINE('',#6642,#1623);
#1309=LINE('',#6646,#1624);
#1310=LINE('',#6650,#1625);
#1311=LINE('',#6657,#1626);
#1312=LINE('',#6661,#1627);
#1313=LINE('',#6665,#1628);
#1314=LINE('',#6670,#1629);
#1315=LINE('',#6672,#1630);
#1316=LINE('',#6674,#1631);
#1317=LINE('',#6675,#1632);
#1318=LINE('',#6678,#1633);
#1319=LINE('',#6680,#1634);
#1320=LINE('',#6681,#1635);
#1321=LINE('',#6684,#1636);
#1322=LINE('',#6686,#1637);
#1323=LINE('',#6687,#1638);
#1324=LINE('',#6690,#1639);
#1325=LINE('',#6692,#1640);
#1326=LINE('',#6693,#1641);
#1327=LINE('',#6696,#1642);
#1328=LINE('',#6698,#1643);
#1329=LINE('',#6699,#1644);
#1330=LINE('',#6701,#1645);
#1331=LINE('',#6702,#1646);
#1332=LINE('',#6710,#1647);
#1333=LINE('',#6716,#1648);
#1334=LINE('',#6732,#1649);
#1335=LINE('',#6753,#1650);
#1336=LINE('',#6778,#1651);
#1337=LINE('',#6779,#1652);
#1338=LINE('',#6781,#1653);
#1339=LINE('',#6783,#1654);
#1340=LINE('',#6788,#1655);
#1341=LINE('',#6791,#1656);
#1342=LINE('',#6793,#1657);
#1343=VECTOR('',#4542,0.21);
#1344=VECTOR('',#4549,0.21);
#1345=VECTOR('',#4556,0.21);
#1346=VECTOR('',#4563,0.21);
#1347=VECTOR('',#4568,1.);
#1348=VECTOR('',#4569,1.);
#1349=VECTOR('',#4570,1.);
#1350=VECTOR('',#4571,1.);
#1351=VECTOR('',#4574,1.);
#1352=VECTOR('',#4575,1.);
#1353=VECTOR('',#4576,1.);
#1354=VECTOR('',#4579,1.);
#1355=VECTOR('',#4580,1.);
#1356=VECTOR('',#4581,1.);
#1357=VECTOR('',#4584,1.);
#1358=VECTOR('',#4585,1.);
#1359=VECTOR('',#4594,1.);
#1360=VECTOR('',#4595,1.);
#1361=VECTOR('',#4596,1.);
#1362=VECTOR('',#4597,1.);
#1363=VECTOR('',#4600,1.);
#1364=VECTOR('',#4601,1.);
#1365=VECTOR('',#4602,1.);
#1366=VECTOR('',#4605,1.);
#1367=VECTOR('',#4606,1.);
#1368=VECTOR('',#4607,1.);
#1369=VECTOR('',#4610,1.);
#1370=VECTOR('',#4611,1.);
#1371=VECTOR('',#4620,1.);
#1372=VECTOR('',#4621,1.);
#1373=VECTOR('',#4622,1.);
#1374=VECTOR('',#4623,1.);
#1375=VECTOR('',#4626,1.);
#1376=VECTOR('',#4627,1.);
#1377=VECTOR('',#4628,1.);
#1378=VECTOR('',#4631,1.);
#1379=VECTOR('',#4632,1.);
#1380=VECTOR('',#4633,1.);
#1381=VECTOR('',#4636,1.);
#1382=VECTOR('',#4637,1.);
#1383=VECTOR('',#4648,0.21);
#1384=VECTOR('',#4657,0.21);
#1385=VECTOR('',#4666,0.275);
#1386=VECTOR('',#4673,0.275);
#1387=VECTOR('',#4678,1.);
#1388=VECTOR('',#4681,1.);
#1389=VECTOR('',#4686,1.);
#1390=VECTOR('',#4687,1.);
#1391=VECTOR('',#4688,1.);
#1392=VECTOR('',#4689,1.);
#1393=VECTOR('',#4690,1.);
#1394=VECTOR('',#4691,1.);
#1395=VECTOR('',#4692,1.);
#1396=VECTOR('',#4693,1.);
#1397=VECTOR('',#4694,1.);
#1398=VECTOR('',#4695,1.);
#1399=VECTOR('',#4696,1.);
#1400=VECTOR('',#4697,1.);
#1401=VECTOR('',#4698,1.);
#1402=VECTOR('',#4701,1.);
#1403=VECTOR('',#4702,1.);
#1404=VECTOR('',#4705,1.);
#1405=VECTOR('',#4706,1.);
#1406=VECTOR('',#4709,1.);
#1407=VECTOR('',#4710,1.);
#1408=VECTOR('',#4711,1.);
#1409=VECTOR('',#4714,1.);
#1410=VECTOR('',#4715,1.);
#1411=VECTOR('',#4718,1.);
#1412=VECTOR('',#4719,1.);
#1413=VECTOR('',#4722,1.);
#1414=VECTOR('',#4725,1.);
#1415=VECTOR('',#4726,1.);
#1416=VECTOR('',#4729,1.);
#1417=VECTOR('',#4730,1.);
#1418=VECTOR('',#4733,1.);
#1419=VECTOR('',#4734,1.);
#1420=VECTOR('',#4737,1.);
#1421=VECTOR('',#4738,1.);
#1422=VECTOR('',#4741,1.);
#1423=VECTOR('',#4742,1.);
#1424=VECTOR('',#4745,1.);
#1425=VECTOR('',#4746,1.);
#1426=VECTOR('',#4749,1.);
#1427=VECTOR('',#4756,1.);
#1428=VECTOR('',#4763,1.);
#1429=VECTOR('',#4766,1.);
#1430=VECTOR('',#4769,1.);
#1431=VECTOR('',#4776,1.);
#1432=VECTOR('',#4779,1.);
#1433=VECTOR('',#4782,1.);
#1434=VECTOR('',#4783,1.);
#1435=VECTOR('',#4784,1.);
#1436=VECTOR('',#4785,1.);
#1437=VECTOR('',#4786,1.);
#1438=VECTOR('',#4789,1.);
#1439=VECTOR('',#4790,1.);
#1440=VECTOR('',#4791,1.);
#1441=VECTOR('',#4792,1.);
#1442=VECTOR('',#4793,1.);
#1443=VECTOR('',#4798,0.275);
#1444=VECTOR('',#4803,0.275);
#1445=VECTOR('',#4808,1.);
#1446=VECTOR('',#4811,1.);
#1447=VECTOR('',#4814,1.);
#1448=VECTOR('',#4815,1.);
#1449=VECTOR('',#4816,1.);
#1450=VECTOR('',#4819,1.);
#1451=VECTOR('',#4822,1.);
#1452=VECTOR('',#4823,1.);
#1453=VECTOR('',#4834,0.21);
#1454=VECTOR('',#4843,0.21);
#1455=VECTOR('',#4852,0.275);
#1456=VECTOR('',#4859,0.275);
#1457=VECTOR('',#4864,1.);
#1458=VECTOR('',#4867,1.);
#1459=VECTOR('',#4872,1.);
#1460=VECTOR('',#4873,1.);
#1461=VECTOR('',#4874,1.);
#1462=VECTOR('',#4875,1.);
#1463=VECTOR('',#4876,1.);
#1464=VECTOR('',#4877,1.);
#1465=VECTOR('',#4878,1.);
#1466=VECTOR('',#4879,1.);
#1467=VECTOR('',#4880,1.);
#1468=VECTOR('',#4881,1.);
#1469=VECTOR('',#4882,1.);
#1470=VECTOR('',#4883,1.);
#1471=VECTOR('',#4884,1.);
#1472=VECTOR('',#4887,1.);
#1473=VECTOR('',#4888,1.);
#1474=VECTOR('',#4891,1.);
#1475=VECTOR('',#4892,1.);
#1476=VECTOR('',#4895,1.);
#1477=VECTOR('',#4896,1.);
#1478=VECTOR('',#4897,1.);
#1479=VECTOR('',#4900,1.);
#1480=VECTOR('',#4901,1.);
#1481=VECTOR('',#4904,1.);
#1482=VECTOR('',#4905,1.);
#1483=VECTOR('',#4908,1.);
#1484=VECTOR('',#4911,1.);
#1485=VECTOR('',#4912,1.);
#1486=VECTOR('',#4915,1.);
#1487=VECTOR('',#4916,1.);
#1488=VECTOR('',#4919,1.);
#1489=VECTOR('',#4920,1.);
#1490=VECTOR('',#4923,1.);
#1491=VECTOR('',#4924,1.);
#1492=VECTOR('',#4927,1.);
#1493=VECTOR('',#4928,1.);
#1494=VECTOR('',#4931,1.);
#1495=VECTOR('',#4932,1.);
#1496=VECTOR('',#4935,1.);
#1497=VECTOR('',#4942,1.);
#1498=VECTOR('',#4949,1.);
#1499=VECTOR('',#4952,1.);
#1500=VECTOR('',#4955,1.);
#1501=VECTOR('',#4962,1.);
#1502=VECTOR('',#4965,1.);
#1503=VECTOR('',#4968,1.);
#1504=VECTOR('',#4969,1.);
#1505=VECTOR('',#4970,1.);
#1506=VECTOR('',#4971,1.);
#1507=VECTOR('',#4972,1.);
#1508=VECTOR('',#4975,1.);
#1509=VECTOR('',#4976,1.);
#1510=VECTOR('',#4977,1.);
#1511=VECTOR('',#4978,1.);
#1512=VECTOR('',#4979,1.);
#1513=VECTOR('',#4984,0.275);
#1514=VECTOR('',#4989,0.275);
#1515=VECTOR('',#4994,1.);
#1516=VECTOR('',#4997,1.);
#1517=VECTOR('',#5000,1.);
#1518=VECTOR('',#5001,1.);
#1519=VECTOR('',#5002,1.);
#1520=VECTOR('',#5005,1.);
#1521=VECTOR('',#5008,1.);
#1522=VECTOR('',#5009,1.);
#1523=VECTOR('',#5020,0.93);
#1524=VECTOR('',#5031,0.79);
#1525=VECTOR('',#5036,1.3);
#1526=VECTOR('',#5049,0.44);
#1527=VECTOR('',#5056,0.44);
#1528=VECTOR('',#5063,0.44);
#1529=VECTOR('',#5070,0.44);
#1530=VECTOR('',#5083,3.5);
#1531=VECTOR('',#5088,0.79);
#1532=VECTOR('',#5093,1.5);
#1533=VECTOR('',#5106,0.93);
#1534=VECTOR('',#5115,0.79);
#1535=VECTOR('',#5122,1.3);
#1536=VECTOR('',#5135,0.44);
#1537=VECTOR('',#5142,0.44);
#1538=VECTOR('',#5149,0.44);
#1539=VECTOR('',#5156,0.44);
#1540=VECTOR('',#5167,3.5);
#1541=VECTOR('',#5174,0.79);
#1542=VECTOR('',#5181,1.5);
#1543=VECTOR('',#5192,0.79);
#1544=VECTOR('',#5199,2.2);
#1545=VECTOR('',#5210,1.);
#1546=VECTOR('',#5211,1.);
#1547=VECTOR('',#5212,1.);
#1548=VECTOR('',#5213,1.);
#1549=VECTOR('',#5216,1.);
#1550=VECTOR('',#5217,1.);
#1551=VECTOR('',#5218,1.);
#1552=VECTOR('',#5221,1.);
#1553=VECTOR('',#5222,1.);
#1554=VECTOR('',#5223,1.);
#1555=VECTOR('',#5226,1.);
#1556=VECTOR('',#5227,1.);
#1557=VECTOR('',#5228,1.);
#1558=VECTOR('',#5231,1.);
#1559=VECTOR('',#5232,1.);
#1560=VECTOR('',#5233,1.);
#1561=VECTOR('',#5236,1.);
#1562=VECTOR('',#5237,1.);
#1563=VECTOR('',#5254,0.4);
#1564=VECTOR('',#5259,0.425);
#1565=VECTOR('',#5264,0.41);
#1566=VECTOR('',#5273,0.26);
#1567=VECTOR('',#5276,0.25);
#1568=VECTOR('',#5287,0.4);
#1569=VECTOR('',#5292,0.425);
#1570=VECTOR('',#5297,0.41);
#1571=VECTOR('',#5306,0.26);
#1572=VECTOR('',#5311,0.25);
#1573=VECTOR('',#5316,0.225);
#1574=VECTOR('',#5321,1.);
#1575=VECTOR('',#5322,1.);
#1576=VECTOR('',#5323,1.);
#1577=VECTOR('',#5324,1.);
#1578=VECTOR('',#5327,1.);
#1579=VECTOR('',#5328,1.);
#1580=VECTOR('',#5329,1.);
#1581=VECTOR('',#5332,1.);
#1582=VECTOR('',#5333,1.);
#1583=VECTOR('',#5334,1.);
#1584=VECTOR('',#5337,1.);
#1585=VECTOR('',#5338,1.);
#1586=VECTOR('',#5339,1.);
#1587=VECTOR('',#5342,1.);
#1588=VECTOR('',#5343,1.);
#1589=VECTOR('',#5344,1.);
#1590=VECTOR('',#5347,1.);
#1591=VECTOR('',#5348,1.);
#1592=VECTOR('',#5361,0.79);
#1593=VECTOR('',#5376,0.79);
#1594=VECTOR('',#5387,0.93);
#1595=VECTOR('',#5392,0.93);
#1596=VECTOR('',#5411,1.2);
#1597=VECTOR('',#5422,1.45);
#1598=VECTOR('',#5435,1.45);
#1599=VECTOR('',#5440,1.2);
#1600=VECTOR('',#5445,1.);
#1601=VECTOR('',#5446,1.);
#1602=VECTOR('',#5447,1.);
#1603=VECTOR('',#5448,1.);
#1604=VECTOR('',#5449,1.);
#1605=VECTOR('',#5450,1.);
#1606=VECTOR('',#5455,1.);
#1607=VECTOR('',#5456,1.);
#1608=VECTOR('',#5457,1.);
#1609=VECTOR('',#5458,1.);
#1610=VECTOR('',#5459,1.);
#1611=VECTOR('',#5460,1.);
#1612=VECTOR('',#5465,1.);
#1613=VECTOR('',#5466,1.);
#1614=VECTOR('',#5469,1.);
#1615=VECTOR('',#5472,1.);
#1616=VECTOR('',#5475,1.);
#1617=VECTOR('',#5478,1.);
#1618=VECTOR('',#5483,1.065);
#1619=VECTOR('',#5494,1.025);
#1620=VECTOR('',#5499,1.065);
#1621=VECTOR('',#5504,1.025);
#1622=VECTOR('',#5511,0.79);
#1623=VECTOR('',#5522,0.625);
#1624=VECTOR('',#5527,0.65);
#1625=VECTOR('',#5532,0.635);
#1626=VECTOR('',#5541,0.41);
#1627=VECTOR('',#5546,0.4);
#1628=VECTOR('',#5551,0.36);
#1629=VECTOR('',#5556,1.);
#1630=VECTOR('',#5557,1.);
#1631=VECTOR('',#5558,1.);
#1632=VECTOR('',#5559,1.);
#1633=VECTOR('',#5562,1.);
#1634=VECTOR('',#5563,1.);
#1635=VECTOR('',#5564,1.);
#1636=VECTOR('',#5567,1.);
#1637=VECTOR('',#5568,1.);
#1638=VECTOR('',#5569,1.);
#1639=VECTOR('',#5572,1.);
#1640=VECTOR('',#5573,1.);
#1641=VECTOR('',#5574,1.);
#1642=VECTOR('',#5577,1.);
#1643=VECTOR('',#5578,1.);
#1644=VECTOR('',#5579,1.);
#1645=VECTOR('',#5582,1.);
#1646=VECTOR('',#5583,1.);
#1647=VECTOR('',#5594,0.42);
#1648=VECTOR('',#5601,0.8);
#1649=VECTOR('',#5612,0.734027674973257);
#1650=VECTOR('',#5619,0.734027674973257);
#1651=VECTOR('',#5622,1.);
#1652=VECTOR('',#5623,1.);
#1653=VECTOR('',#5626,1.);
#1654=VECTOR('',#5629,1.);
#1655=VECTOR('',#5634,0.4);
#1656=VECTOR('',#5639,1.);
#1657=VECTOR('',#5642,1.);
#1658=CIRCLE('',#4097,0.21);
#1659=CIRCLE('',#4098,0.21);
#1660=CIRCLE('',#4100,0.21);
#1661=CIRCLE('',#4101,0.21);
#1662=CIRCLE('',#4103,0.21);
#1663=CIRCLE('',#4104,0.21);
#1664=CIRCLE('',#4106,0.21);
#1665=CIRCLE('',#4107,0.21);
#1666=CIRCLE('',#4130,0.21);
#1667=CIRCLE('',#4131,0.21);
#1668=CIRCLE('',#4134,0.21);
#1669=CIRCLE('',#4135,0.21);
#1670=CIRCLE('',#4138,0.275);
#1671=CIRCLE('',#4139,0.275);
#1672=CIRCLE('',#4141,0.275);
#1673=CIRCLE('',#4142,0.275);
#1674=CIRCLE('',#4144,1.31);
#1675=CIRCLE('',#4145,1.31);
#1676=CIRCLE('',#4163,0.475);
#1677=CIRCLE('',#4164,0.275);
#1678=CIRCLE('',#4166,0.475);
#1679=CIRCLE('',#4168,0.475);
#1680=CIRCLE('',#4169,0.275);
#1681=CIRCLE('',#4171,0.475);
#1682=CIRCLE('',#4175,0.275);
#1683=CIRCLE('',#4177,0.275);
#1684=CIRCLE('',#4179,1.31);
#1685=CIRCLE('',#4180,1.31);
#1686=CIRCLE('',#4188,0.21);
#1687=CIRCLE('',#4189,0.21);
#1688=CIRCLE('',#4192,0.21);
#1689=CIRCLE('',#4193,0.21);
#1690=CIRCLE('',#4196,0.275);
#1691=CIRCLE('',#4197,0.275);
#1692=CIRCLE('',#4199,0.275);
#1693=CIRCLE('',#4200,0.275);
#1694=CIRCLE('',#4202,1.31);
#1695=CIRCLE('',#4203,1.31);
#1696=CIRCLE('',#4221,0.475);
#1697=CIRCLE('',#4222,0.275);
#1698=CIRCLE('',#4224,0.475);
#1699=CIRCLE('',#4226,0.475);
#1700=CIRCLE('',#4227,0.275);
#1701=CIRCLE('',#4229,0.475);
#1702=CIRCLE('',#4233,0.275);
#1703=CIRCLE('',#4235,0.275);
#1704=CIRCLE('',#4237,1.31);
#1705=CIRCLE('',#4238,1.31);
#1706=CIRCLE('',#4246,0.93);
#1707=CIRCLE('',#4247,0.93);
#1708=CIRCLE('',#4249,0.79);
#1709=CIRCLE('',#4251,0.79);
#1710=CIRCLE('',#4253,1.3);
#1711=CIRCLE('',#4254,1.3);
#1712=CIRCLE('',#4259,0.44);
#1713=CIRCLE('',#4260,0.44);
#1714=CIRCLE('',#4262,0.44);
#1715=CIRCLE('',#4263,0.44);
#1716=CIRCLE('',#4265,0.44);
#1717=CIRCLE('',#4266,0.44);
#1718=CIRCLE('',#4268,0.44);
#1719=CIRCLE('',#4269,0.44);
#1720=CIRCLE('',#4271,3.5);
#1721=CIRCLE('',#4272,1.5);
#1722=CIRCLE('',#4274,3.5);
#1723=CIRCLE('',#4276,0.79);
#1724=CIRCLE('',#4277,0.79);
#1725=CIRCLE('',#4279,1.5);
#1726=CIRCLE('',#4284,0.93);
#1727=CIRCLE('',#4285,0.93);
#1728=CIRCLE('',#4287,0.79);
#1729=CIRCLE('',#4289,0.79);
#1730=CIRCLE('',#4291,1.3);
#1731=CIRCLE('',#4292,1.3);
#1732=CIRCLE('',#4297,0.44);
#1733=CIRCLE('',#4298,0.44);
#1734=CIRCLE('',#4300,0.44);
#1735=CIRCLE('',#4301,0.44);
#1736=CIRCLE('',#4303,0.44);
#1737=CIRCLE('',#4304,0.44);
#1738=CIRCLE('',#4306,0.44);
#1739=CIRCLE('',#4307,0.44);
#1740=CIRCLE('',#4309,3.5);
#1741=CIRCLE('',#4310,1.5);
#1742=CIRCLE('',#4312,3.5);
#1743=CIRCLE('',#4314,0.79);
#1744=CIRCLE('',#4315,0.79);
#1745=CIRCLE('',#4317,1.5);
#1746=CIRCLE('',#4322,0.79);
#1747=CIRCLE('',#4323,0.79);
#1748=CIRCLE('',#4325,2.2);
#1749=CIRCLE('',#4326,2.2);
#1750=CIRCLE('',#4339,0.24505);
#1751=CIRCLE('',#4341,0.375);
#1752=CIRCLE('',#4343,0.425);
#1753=CIRCLE('',#4345,0.425);
#1754=CIRCLE('',#4347,0.395);
#1755=CIRCLE('',#4349,0.27);
#1756=CIRCLE('',#4351,0.24505);
#1757=CIRCLE('',#4355,0.375);
#1758=CIRCLE('',#4357,0.425);
#1759=CIRCLE('',#4359,0.425);
#1760=CIRCLE('',#4361,0.395);
#1761=CIRCLE('',#4363,0.27);
#1762=CIRCLE('',#4365,0.24505);
#1763=CIRCLE('',#4367,0.24505);
#1764=CIRCLE('',#4369,0.2);
#1765=CIRCLE('',#4382,0.79);
#1766=CIRCLE('',#4383,0.79);
#1767=CIRCLE('',#4384,0.79);
#1768=CIRCLE('',#4386,0.837);
#1769=CIRCLE('',#4387,0.79);
#1770=CIRCLE('',#4388,0.79);
#1771=CIRCLE('',#4390,0.79);
#1772=CIRCLE('',#4392,0.93);
#1773=CIRCLE('',#4394,0.93);
#1774=CIRCLE('',#4396,0.93);
#1775=CIRCLE('',#4397,0.93);
#1776=CIRCLE('',#4400,1.2);
#1777=CIRCLE('',#4401,1.2);
#1778=CIRCLE('',#4402,1.2);
#1779=CIRCLE('',#4403,1.2);
#1780=CIRCLE('',#4406,1.2);
#1781=CIRCLE('',#4408,1.45);
#1782=CIRCLE('',#4410,1.45);
#1783=CIRCLE('',#4413,1.45);
#1784=CIRCLE('',#4414,1.2);
#1785=CIRCLE('',#4416,1.45);
#1786=CIRCLE('',#4421,1.065);
#1787=CIRCLE('',#4423,1.065);
#1788=CIRCLE('',#4431,1.065);
#1789=CIRCLE('',#4433,0.985);
#1790=CIRCLE('',#4434,0.79);
#1791=CIRCLE('',#4437,1.065);
#1792=CIRCLE('',#4439,0.985);
#1793=CIRCLE('',#4441,0.79);
#1794=CIRCLE('',#4445,0.6);
#1795=CIRCLE('',#4447,0.65);
#1796=CIRCLE('',#4449,0.65);
#1797=CIRCLE('',#4451,0.62);
#1798=CIRCLE('',#4453,0.42);
#1799=CIRCLE('',#4455,0.3933);
#1800=CIRCLE('',#4457,0.3933);
#1801=CIRCLE('',#4459,0.32);
#1802=CIRCLE('',#4471,0.42);
#1803=CIRCLE('',#4472,0.42);
#1804=CIRCLE('',#4474,0.8);
#1805=CIRCLE('',#4475,0.8);
#1806=CIRCLE('',#4480,0.6175);
#1807=CIRCLE('',#4482,0.6175);
#1808=CIRCLE('',#4487,0.338975);
#1809=CIRCLE('',#4488,0.338975);
#1810=VERTEX_POINT('',#5732);
#1811=VERTEX_POINT('',#5734);
#1812=VERTEX_POINT('',#5738);
#1813=VERTEX_POINT('',#5740);
#1814=VERTEX_POINT('',#5744);
#1815=VERTEX_POINT('',#5746);
#1816=VERTEX_POINT('',#5750);
#1817=VERTEX_POINT('',#5752);
#1818=VERTEX_POINT('',#5756);
#1819=VERTEX_POINT('',#5757);
#1820=VERTEX_POINT('',#5759);
#1821=VERTEX_POINT('',#5761);
#1822=VERTEX_POINT('',#5765);
#1823=VERTEX_POINT('',#5767);
#1824=VERTEX_POINT('',#5771);
#1825=VERTEX_POINT('',#5773);
#1826=VERTEX_POINT('',#5783);
#1827=VERTEX_POINT('',#5784);
#1828=VERTEX_POINT('',#5786);
#1829=VERTEX_POINT('',#5788);
#1830=VERTEX_POINT('',#5792);
#1831=VERTEX_POINT('',#5794);
#1832=VERTEX_POINT('',#5798);
#1833=VERTEX_POINT('',#5800);
#1834=VERTEX_POINT('',#5810);
#1835=VERTEX_POINT('',#5811);
#1836=VERTEX_POINT('',#5813);
#1837=VERTEX_POINT('',#5815);
#1838=VERTEX_POINT('',#5819);
#1839=VERTEX_POINT('',#5821);
#1840=VERTEX_POINT('',#5825);
#1841=VERTEX_POINT('',#5827);
#1842=VERTEX_POINT('',#5837);
#1843=VERTEX_POINT('',#5839);
#1844=VERTEX_POINT('',#5844);
#1845=VERTEX_POINT('',#5846);
#1846=VERTEX_POINT('',#5851);
#1847=VERTEX_POINT('',#5853);
#1848=VERTEX_POINT('',#5857);
#1849=VERTEX_POINT('',#5859);
#1850=VERTEX_POINT('',#5863);
#1851=VERTEX_POINT('',#5864);
#1852=VERTEX_POINT('',#5866);
#1853=VERTEX_POINT('',#5868);
#1854=VERTEX_POINT('',#5872);
#1855=VERTEX_POINT('',#5874);
#1856=VERTEX_POINT('',#5876);
#1857=VERTEX_POINT('',#5878);
#1858=VERTEX_POINT('',#5880);
#1859=VERTEX_POINT('',#5882);
#1860=VERTEX_POINT('',#5884);
#1861=VERTEX_POINT('',#5886);
#1862=VERTEX_POINT('',#5888);
#1863=VERTEX_POINT('',#5890);
#1864=VERTEX_POINT('',#5892);
#1865=VERTEX_POINT('',#5894);
#1866=VERTEX_POINT('',#5898);
#1867=VERTEX_POINT('',#5902);
#1868=VERTEX_POINT('',#5906);
#1869=VERTEX_POINT('',#5907);
#1870=VERTEX_POINT('',#5912);
#1871=VERTEX_POINT('',#5916);
#1872=VERTEX_POINT('',#5922);
#1873=VERTEX_POINT('',#5926);
#1874=VERTEX_POINT('',#5930);
#1875=VERTEX_POINT('',#5934);
#1876=VERTEX_POINT('',#5938);
#1877=VERTEX_POINT('',#5942);
#1878=VERTEX_POINT('',#5950);
#1879=VERTEX_POINT('',#5951);
#1880=VERTEX_POINT('',#5954);
#1881=VERTEX_POINT('',#5957);
#1882=VERTEX_POINT('',#5959);
#1883=VERTEX_POINT('',#5963);
#1884=VERTEX_POINT('',#5964);
#1885=VERTEX_POINT('',#5967);
#1886=VERTEX_POINT('',#5970);
#1887=VERTEX_POINT('',#5972);
#1888=VERTEX_POINT('',#5976);
#1889=VERTEX_POINT('',#5978);
#1890=VERTEX_POINT('',#5980);
#1891=VERTEX_POINT('',#5982);
#1892=VERTEX_POINT('',#5986);
#1893=VERTEX_POINT('',#5988);
#1894=VERTEX_POINT('',#5990);
#1895=VERTEX_POINT('',#5992);
#1896=VERTEX_POINT('',#5996);
#1897=VERTEX_POINT('',#6000);
#1898=VERTEX_POINT('',#6004);
#1899=VERTEX_POINT('',#6005);
#1900=VERTEX_POINT('',#6007);
#1901=VERTEX_POINT('',#6009);
#1902=VERTEX_POINT('',#6025);
#1903=VERTEX_POINT('',#6027);
#1904=VERTEX_POINT('',#6032);
#1905=VERTEX_POINT('',#6034);
#1906=VERTEX_POINT('',#6039);
#1907=VERTEX_POINT('',#6041);
#1908=VERTEX_POINT('',#6045);
#1909=VERTEX_POINT('',#6047);
#1910=VERTEX_POINT('',#6051);
#1911=VERTEX_POINT('',#6052);
#1912=VERTEX_POINT('',#6054);
#1913=VERTEX_POINT('',#6056);
#1914=VERTEX_POINT('',#6060);
#1915=VERTEX_POINT('',#6062);
#1916=VERTEX_POINT('',#6064);
#1917=VERTEX_POINT('',#6066);
#1918=VERTEX_POINT('',#6068);
#1919=VERTEX_POINT('',#6070);
#1920=VERTEX_POINT('',#6072);
#1921=VERTEX_POINT('',#6074);
#1922=VERTEX_POINT('',#6076);
#1923=VERTEX_POINT('',#6078);
#1924=VERTEX_POINT('',#6080);
#1925=VERTEX_POINT('',#6082);
#1926=VERTEX_POINT('',#6086);
#1927=VERTEX_POINT('',#6090);
#1928=VERTEX_POINT('',#6094);
#1929=VERTEX_POINT('',#6095);
#1930=VERTEX_POINT('',#6100);
#1931=VERTEX_POINT('',#6104);
#1932=VERTEX_POINT('',#6110);
#1933=VERTEX_POINT('',#6114);
#1934=VERTEX_POINT('',#6118);
#1935=VERTEX_POINT('',#6122);
#1936=VERTEX_POINT('',#6126);
#1937=VERTEX_POINT('',#6130);
#1938=VERTEX_POINT('',#6138);
#1939=VERTEX_POINT('',#6139);
#1940=VERTEX_POINT('',#6142);
#1941=VERTEX_POINT('',#6145);
#1942=VERTEX_POINT('',#6147);
#1943=VERTEX_POINT('',#6151);
#1944=VERTEX_POINT('',#6152);
#1945=VERTEX_POINT('',#6155);
#1946=VERTEX_POINT('',#6158);
#1947=VERTEX_POINT('',#6160);
#1948=VERTEX_POINT('',#6164);
#1949=VERTEX_POINT('',#6166);
#1950=VERTEX_POINT('',#6168);
#1951=VERTEX_POINT('',#6170);
#1952=VERTEX_POINT('',#6174);
#1953=VERTEX_POINT('',#6176);
#1954=VERTEX_POINT('',#6178);
#1955=VERTEX_POINT('',#6180);
#1956=VERTEX_POINT('',#6184);
#1957=VERTEX_POINT('',#6188);
#1958=VERTEX_POINT('',#6192);
#1959=VERTEX_POINT('',#6193);
#1960=VERTEX_POINT('',#6195);
#1961=VERTEX_POINT('',#6197);
#1962=VERTEX_POINT('',#6213);
#1963=VERTEX_POINT('',#6215);
#1964=VERTEX_POINT('',#6219);
#1965=VERTEX_POINT('',#6222);
#1966=VERTEX_POINT('',#6226);
#1967=VERTEX_POINT('',#6228);
#1968=VERTEX_POINT('',#6235);
#1969=VERTEX_POINT('',#6237);
#1970=VERTEX_POINT('',#6241);
#1971=VERTEX_POINT('',#6243);
#1972=VERTEX_POINT('',#6247);
#1973=VERTEX_POINT('',#6249);
#1974=VERTEX_POINT('',#6253);
#1975=VERTEX_POINT('',#6255);
#1976=VERTEX_POINT('',#6259);
#1977=VERTEX_POINT('',#6261);
#1978=VERTEX_POINT('',#6264);
#1979=VERTEX_POINT('',#6268);
#1980=VERTEX_POINT('',#6270);
#1981=VERTEX_POINT('',#6274);
#1982=VERTEX_POINT('',#6281);
#1983=VERTEX_POINT('',#6283);
#1984=VERTEX_POINT('',#6287);
#1985=VERTEX_POINT('',#6290);
#1986=VERTEX_POINT('',#6294);
#1987=VERTEX_POINT('',#6296);
#1988=VERTEX_POINT('',#6303);
#1989=VERTEX_POINT('',#6305);
#1990=VERTEX_POINT('',#6309);
#1991=VERTEX_POINT('',#6311);
#1992=VERTEX_POINT('',#6315);
#1993=VERTEX_POINT('',#6317);
#1994=VERTEX_POINT('',#6321);
#1995=VERTEX_POINT('',#6323);
#1996=VERTEX_POINT('',#6327);
#1997=VERTEX_POINT('',#6329);
#1998=VERTEX_POINT('',#6332);
#1999=VERTEX_POINT('',#6336);
#2000=VERTEX_POINT('',#6338);
#2001=VERTEX_POINT('',#6342);
#2002=VERTEX_POINT('',#6349);
#2003=VERTEX_POINT('',#6351);
#2004=VERTEX_POINT('',#6355);
#2005=VERTEX_POINT('',#6357);
#2006=VERTEX_POINT('',#6364);
#2007=VERTEX_POINT('',#6365);
#2008=VERTEX_POINT('',#6367);
#2009=VERTEX_POINT('',#6369);
#2010=VERTEX_POINT('',#6373);
#2011=VERTEX_POINT('',#6375);
#2012=VERTEX_POINT('',#6379);
#2013=VERTEX_POINT('',#6381);
#2014=VERTEX_POINT('',#6385);
#2015=VERTEX_POINT('',#6387);
#2016=VERTEX_POINT('',#6391);
#2017=VERTEX_POINT('',#6393);
#2018=VERTEX_POINT('',#6402);
#2019=VERTEX_POINT('',#6405);
#2020=VERTEX_POINT('',#6408);
#2021=VERTEX_POINT('',#6412);
#2022=VERTEX_POINT('',#6416);
#2023=VERTEX_POINT('',#6420);
#2024=VERTEX_POINT('',#6423);
#2025=VERTEX_POINT('',#6430);
#2026=VERTEX_POINT('',#6433);
#2027=VERTEX_POINT('',#6437);
#2028=VERTEX_POINT('',#6441);
#2029=VERTEX_POINT('',#6445);
#2030=VERTEX_POINT('',#6448);
#2031=VERTEX_POINT('',#6452);
#2032=VERTEX_POINT('',#6456);
#2033=VERTEX_POINT('',#6461);
#2034=VERTEX_POINT('',#6462);
#2035=VERTEX_POINT('',#6464);
#2036=VERTEX_POINT('',#6466);
#2037=VERTEX_POINT('',#6470);
#2038=VERTEX_POINT('',#6472);
#2039=VERTEX_POINT('',#6476);
#2040=VERTEX_POINT('',#6478);
#2041=VERTEX_POINT('',#6482);
#2042=VERTEX_POINT('',#6484);
#2043=VERTEX_POINT('',#6488);
#2044=VERTEX_POINT('',#6490);
#2045=VERTEX_POINT('',#6500);
#2046=VERTEX_POINT('',#6501);
#2047=VERTEX_POINT('',#6503);
#2048=VERTEX_POINT('',#6505);
#2049=VERTEX_POINT('',#6510);
#2050=VERTEX_POINT('',#6511);
#2051=VERTEX_POINT('',#6513);
#2052=VERTEX_POINT('',#6517);
#2053=VERTEX_POINT('',#6521);
#2054=VERTEX_POINT('',#6524);
#2055=VERTEX_POINT('',#6528);
#2056=VERTEX_POINT('',#6530);
#2057=VERTEX_POINT('',#6535);
#2058=VERTEX_POINT('',#6536);
#2059=VERTEX_POINT('',#6538);
#2060=VERTEX_POINT('',#6540);
#2061=VERTEX_POINT('',#6545);
#2062=VERTEX_POINT('',#6549);
#2063=VERTEX_POINT('',#6552);
#2064=VERTEX_POINT('',#6557);
#2065=VERTEX_POINT('',#6559);
#2066=VERTEX_POINT('',#6562);
#2067=VERTEX_POINT('',#6570);
#2068=VERTEX_POINT('',#6571);
#2069=VERTEX_POINT('',#6573);
#2070=VERTEX_POINT('',#6575);
#2071=VERTEX_POINT('',#6577);
#2072=VERTEX_POINT('',#6579);
#2073=VERTEX_POINT('',#6582);
#2074=VERTEX_POINT('',#6585);
#2075=VERTEX_POINT('',#6586);
#2076=VERTEX_POINT('',#6588);
#2077=VERTEX_POINT('',#6590);
#2078=VERTEX_POINT('',#6592);
#2079=VERTEX_POINT('',#6594);
#2080=VERTEX_POINT('',#6597);
#2081=VERTEX_POINT('',#6612);
#2082=VERTEX_POINT('',#6616);
#2083=VERTEX_POINT('',#6618);
#2084=VERTEX_POINT('',#6623);
#2085=VERTEX_POINT('',#6627);
#2086=VERTEX_POINT('',#6631);
#2087=VERTEX_POINT('',#6637);
#2088=VERTEX_POINT('',#6640);
#2089=VERTEX_POINT('',#6644);
#2090=VERTEX_POINT('',#6648);
#2091=VERTEX_POINT('',#6652);
#2092=VERTEX_POINT('',#6655);
#2093=VERTEX_POINT('',#6659);
#2094=VERTEX_POINT('',#6663);
#2095=VERTEX_POINT('',#6668);
#2096=VERTEX_POINT('',#6669);
#2097=VERTEX_POINT('',#6671);
#2098=VERTEX_POINT('',#6673);
#2099=VERTEX_POINT('',#6677);
#2100=VERTEX_POINT('',#6679);
#2101=VERTEX_POINT('',#6683);
#2102=VERTEX_POINT('',#6685);
#2103=VERTEX_POINT('',#6689);
#2104=VERTEX_POINT('',#6691);
#2105=VERTEX_POINT('',#6695);
#2106=VERTEX_POINT('',#6697);
#2107=VERTEX_POINT('',#6707);
#2108=VERTEX_POINT('',#6709);
#2109=VERTEX_POINT('',#6713);
#2110=VERTEX_POINT('',#6715);
#2111=VERTEX_POINT('',#6722);
#2112=VERTEX_POINT('',#6723);
#2113=VERTEX_POINT('',#6727);
#2114=VERTEX_POINT('',#6731);
#2115=VERTEX_POINT('',#6734);
#2116=VERTEX_POINT('',#6738);
#2117=VERTEX_POINT('',#6742);
#2118=VERTEX_POINT('',#6750);
#2119=VERTEX_POINT('',#6752);
#2120=VERTEX_POINT('',#6754);
#2121=VERTEX_POINT('',#6758);
#2122=VERTEX_POINT('',#6762);
#2123=VERTEX_POINT('',#6766);
#2124=VERTEX_POINT('',#6770);
#2125=VERTEX_POINT('',#6785);
#2126=VERTEX_POINT('',#6787);
#2127=EDGE_CURVE('',#1810,#1810,#1658,.T.);
#2128=EDGE_CURVE('',#1810,#1811,#1028,.T.);
#2129=EDGE_CURVE('',#1811,#1811,#1659,.T.);
#2130=EDGE_CURVE('',#1812,#1812,#1660,.T.);
#2131=EDGE_CURVE('',#1812,#1813,#1029,.T.);
#2132=EDGE_CURVE('',#1813,#1813,#1661,.T.);
#2133=EDGE_CURVE('',#1814,#1814,#1662,.T.);
#2134=EDGE_CURVE('',#1814,#1815,#1030,.T.);
#2135=EDGE_CURVE('',#1815,#1815,#1663,.T.);
#2136=EDGE_CURVE('',#1816,#1816,#1664,.T.);
#2137=EDGE_CURVE('',#1816,#1817,#1031,.T.);
#2138=EDGE_CURVE('',#1817,#1817,#1665,.T.);
#2139=EDGE_CURVE('',#1818,#1819,#1032,.T.);
#2140=EDGE_CURVE('',#1819,#1820,#1033,.T.);
#2141=EDGE_CURVE('',#1821,#1820,#1034,.T.);
#2142=EDGE_CURVE('',#1818,#1821,#1035,.T.);
#2143=EDGE_CURVE('',#1822,#1818,#1036,.T.);
#2144=EDGE_CURVE('',#1823,#1821,#1037,.T.);
#2145=EDGE_CURVE('',#1822,#1823,#1038,.T.);
#2146=EDGE_CURVE('',#1824,#1822,#1039,.T.);
#2147=EDGE_CURVE('',#1825,#1823,#1040,.T.);
#2148=EDGE_CURVE('',#1824,#1825,#1041,.T.);
#2149=EDGE_CURVE('',#1819,#1824,#1042,.T.);
#2150=EDGE_CURVE('',#1820,#1825,#1043,.T.);
#2151=EDGE_CURVE('',#1826,#1827,#1044,.T.);
#2152=EDGE_CURVE('',#1827,#1828,#1045,.T.);
#2153=EDGE_CURVE('',#1829,#1828,#1046,.T.);
#2154=EDGE_CURVE('',#1826,#1829,#1047,.T.);
#2155=EDGE_CURVE('',#1830,#1826,#1048,.T.);
#2156=EDGE_CURVE('',#1831,#1829,#1049,.T.);
#2157=EDGE_CURVE('',#1830,#1831,#1050,.T.);
#2158=EDGE_CURVE('',#1832,#1830,#1051,.T.);
#2159=EDGE_CURVE('',#1833,#1831,#1052,.T.);
#2160=EDGE_CURVE('',#1832,#1833,#1053,.T.);
#2161=EDGE_CURVE('',#1827,#1832,#1054,.T.);
#2162=EDGE_CURVE('',#1828,#1833,#1055,.T.);
#2163=EDGE_CURVE('',#1834,#1835,#1056,.T.);
#2164=EDGE_CURVE('',#1835,#1836,#1057,.T.);
#2165=EDGE_CURVE('',#1837,#1836,#1058,.T.);
#2166=EDGE_CURVE('',#1834,#1837,#1059,.T.);
#2167=EDGE_CURVE('',#1838,#1834,#1060,.T.);
#2168=EDGE_CURVE('',#1839,#1837,#1061,.T.);
#2169=EDGE_CURVE('',#1838,#1839,#1062,.T.);
#2170=EDGE_CURVE('',#1840,#1838,#1063,.T.);
#2171=EDGE_CURVE('',#1841,#1839,#1064,.T.);
#2172=EDGE_CURVE('',#1840,#1841,#1065,.T.);
#2173=EDGE_CURVE('',#1835,#1840,#1066,.T.);
#2174=EDGE_CURVE('',#1836,#1841,#1067,.T.);
#2175=EDGE_CURVE('',#1842,#1842,#1666,.T.);
#2176=EDGE_CURVE('',#1842,#1843,#1068,.T.);
#2177=EDGE_CURVE('',#1843,#1843,#1667,.T.);
#2178=EDGE_CURVE('',#1844,#1844,#1668,.T.);
#2179=EDGE_CURVE('',#1844,#1845,#1069,.T.);
#2180=EDGE_CURVE('',#1845,#1845,#1669,.T.);
#2181=EDGE_CURVE('',#1846,#1846,#1670,.T.);
#2182=EDGE_CURVE('',#1846,#1847,#1070,.T.);
#2183=EDGE_CURVE('',#1847,#1847,#1671,.T.);
#2184=EDGE_CURVE('',#1848,#1848,#1672,.T.);
#2185=EDGE_CURVE('',#1848,#1849,#1071,.T.);
#2186=EDGE_CURVE('',#1849,#1849,#1673,.T.);
#2187=EDGE_CURVE('',#1850,#1851,#1072,.T.);
#2188=EDGE_CURVE('',#1852,#1850,#1674,.T.);
#2189=EDGE_CURVE('',#1853,#1852,#1073,.T.);
#2190=EDGE_CURVE('',#1851,#1853,#1675,.T.);
#2191=EDGE_CURVE('',#1850,#1854,#1074,.T.);
#2192=EDGE_CURVE('',#1854,#1855,#1075,.T.);
#2193=EDGE_CURVE('',#1855,#1856,#1076,.T.);
#2194=EDGE_CURVE('',#1856,#1857,#1077,.T.);
#2195=EDGE_CURVE('',#1857,#1858,#1078,.T.);
#2196=EDGE_CURVE('',#1858,#1859,#1079,.T.);
#2197=EDGE_CURVE('',#1859,#1860,#1080,.T.);
#2198=EDGE_CURVE('',#1860,#1861,#1081,.T.);
#2199=EDGE_CURVE('',#1861,#1862,#1082,.T.);
#2200=EDGE_CURVE('',#1862,#1863,#1083,.T.);
#2201=EDGE_CURVE('',#1863,#1864,#1084,.T.);
#2202=EDGE_CURVE('',#1864,#1865,#1085,.T.);
#2203=EDGE_CURVE('',#1865,#1852,#1086,.T.);
#2204=EDGE_CURVE('',#1851,#1866,#1087,.T.);
#2205=EDGE_CURVE('',#1866,#1854,#1088,.T.);
#2206=EDGE_CURVE('',#1867,#1865,#1089,.T.);
#2207=EDGE_CURVE('',#1867,#1853,#1090,.T.);
#2208=EDGE_CURVE('',#1868,#1869,#1091,.T.);
#2209=EDGE_CURVE('',#1869,#1858,#1092,.T.);
#2210=EDGE_CURVE('',#1868,#1857,#1093,.T.);
#2211=EDGE_CURVE('',#1870,#1868,#1094,.T.);
#2212=EDGE_CURVE('',#1870,#1856,#1095,.T.);
#2213=EDGE_CURVE('',#1871,#1870,#1096,.T.);
#2214=EDGE_CURVE('',#1871,#1855,#1097,.T.);
#2215=EDGE_CURVE('',#1866,#1871,#1098,.T.);
#2216=EDGE_CURVE('',#1872,#1867,#1099,.T.);
#2217=EDGE_CURVE('',#1872,#1864,#1100,.T.);
#2218=EDGE_CURVE('',#1873,#1872,#1101,.T.);
#2219=EDGE_CURVE('',#1873,#1863,#1102,.T.);
#2220=EDGE_CURVE('',#1874,#1873,#1103,.T.);
#2221=EDGE_CURVE('',#1874,#1862,#1104,.T.);
#2222=EDGE_CURVE('',#1875,#1874,#1105,.T.);
#2223=EDGE_CURVE('',#1875,#1861,#1106,.T.);
#2224=EDGE_CURVE('',#1876,#1875,#1107,.T.);
#2225=EDGE_CURVE('',#1876,#1860,#1108,.T.);
#2226=EDGE_CURVE('',#1877,#1876,#1109,.T.);
#2227=EDGE_CURVE('',#1877,#1859,#1110,.T.);
#2228=EDGE_CURVE('',#1869,#1877,#1111,.T.);
#2229=EDGE_CURVE('',#1878,#1879,#1112,.T.);
#2230=EDGE_CURVE('',#1878,#1879,#1676,.T.);
#2231=EDGE_CURVE('',#1880,#1880,#1677,.T.);
#2232=EDGE_CURVE('',#1881,#1878,#1113,.T.);
#2233=EDGE_CURVE('',#1882,#1881,#1678,.T.);
#2234=EDGE_CURVE('',#1879,#1882,#1114,.T.);
#2235=EDGE_CURVE('',#1883,#1884,#1115,.T.);
#2236=EDGE_CURVE('',#1883,#1884,#1679,.T.);
#2237=EDGE_CURVE('',#1885,#1885,#1680,.T.);
#2238=EDGE_CURVE('',#1886,#1883,#1116,.T.);
#2239=EDGE_CURVE('',#1887,#1886,#1681,.T.);
#2240=EDGE_CURVE('',#1884,#1887,#1117,.T.);
#2241=EDGE_CURVE('',#1888,#1882,#1118,.T.);
#2242=EDGE_CURVE('',#1889,#1888,#1119,.T.);
#2243=EDGE_CURVE('',#1889,#1890,#1120,.T.);
#2244=EDGE_CURVE('',#1890,#1891,#1121,.T.);
#2245=EDGE_CURVE('',#1881,#1891,#1122,.T.);
#2246=EDGE_CURVE('',#1892,#1887,#1123,.T.);
#2247=EDGE_CURVE('',#1893,#1892,#1124,.T.);
#2248=EDGE_CURVE('',#1893,#1894,#1125,.T.);
#2249=EDGE_CURVE('',#1894,#1895,#1126,.T.);
#2250=EDGE_CURVE('',#1886,#1895,#1127,.T.);
#2251=EDGE_CURVE('',#1896,#1896,#1682,.T.);
#2252=EDGE_CURVE('',#1896,#1880,#1128,.T.);
#2253=EDGE_CURVE('',#1897,#1897,#1683,.T.);
#2254=EDGE_CURVE('',#1897,#1885,#1129,.T.);
#2255=EDGE_CURVE('',#1898,#1899,#1684,.T.);
#2256=EDGE_CURVE('',#1900,#1898,#1130,.T.);
#2257=EDGE_CURVE('',#1901,#1900,#1685,.T.);
#2258=EDGE_CURVE('',#1899,#1901,#1131,.T.);
#2259=EDGE_CURVE('',#1900,#1893,#1132,.T.);
#2260=EDGE_CURVE('',#1891,#1892,#1133,.T.);
#2261=EDGE_CURVE('',#1890,#1901,#1134,.T.);
#2262=EDGE_CURVE('',#1894,#1898,#1135,.T.);
#2263=EDGE_CURVE('',#1899,#1889,#1136,.T.);
#2264=EDGE_CURVE('',#1895,#1888,#1137,.T.);
#2265=EDGE_CURVE('',#1902,#1902,#1686,.T.);
#2266=EDGE_CURVE('',#1902,#1903,#1138,.T.);
#2267=EDGE_CURVE('',#1903,#1903,#1687,.T.);
#2268=EDGE_CURVE('',#1904,#1904,#1688,.T.);
#2269=EDGE_CURVE('',#1904,#1905,#1139,.T.);
#2270=EDGE_CURVE('',#1905,#1905,#1689,.T.);
#2271=EDGE_CURVE('',#1906,#1906,#1690,.T.);
#2272=EDGE_CURVE('',#1906,#1907,#1140,.T.);
#2273=EDGE_CURVE('',#1907,#1907,#1691,.T.);
#2274=EDGE_CURVE('',#1908,#1908,#1692,.T.);
#2275=EDGE_CURVE('',#1908,#1909,#1141,.T.);
#2276=EDGE_CURVE('',#1909,#1909,#1693,.T.);
#2277=EDGE_CURVE('',#1910,#1911,#1142,.T.);
#2278=EDGE_CURVE('',#1912,#1910,#1694,.T.);
#2279=EDGE_CURVE('',#1913,#1912,#1143,.T.);
#2280=EDGE_CURVE('',#1911,#1913,#1695,.T.);
#2281=EDGE_CURVE('',#1910,#1914,#1144,.T.);
#2282=EDGE_CURVE('',#1914,#1915,#1145,.T.);
#2283=EDGE_CURVE('',#1915,#1916,#1146,.T.);
#2284=EDGE_CURVE('',#1916,#1917,#1147,.T.);
#2285=EDGE_CURVE('',#1917,#1918,#1148,.T.);
#2286=EDGE_CURVE('',#1918,#1919,#1149,.T.);
#2287=EDGE_CURVE('',#1919,#1920,#1150,.T.);
#2288=EDGE_CURVE('',#1920,#1921,#1151,.T.);
#2289=EDGE_CURVE('',#1921,#1922,#1152,.T.);
#2290=EDGE_CURVE('',#1922,#1923,#1153,.T.);
#2291=EDGE_CURVE('',#1923,#1924,#1154,.T.);
#2292=EDGE_CURVE('',#1924,#1925,#1155,.T.);
#2293=EDGE_CURVE('',#1925,#1912,#1156,.T.);
#2294=EDGE_CURVE('',#1911,#1926,#1157,.T.);
#2295=EDGE_CURVE('',#1926,#1914,#1158,.T.);
#2296=EDGE_CURVE('',#1927,#1925,#1159,.T.);
#2297=EDGE_CURVE('',#1927,#1913,#1160,.T.);
#2298=EDGE_CURVE('',#1928,#1929,#1161,.T.);
#2299=EDGE_CURVE('',#1929,#1918,#1162,.T.);
#2300=EDGE_CURVE('',#1928,#1917,#1163,.T.);
#2301=EDGE_CURVE('',#1930,#1928,#1164,.T.);
#2302=EDGE_CURVE('',#1930,#1916,#1165,.T.);
#2303=EDGE_CURVE('',#1931,#1930,#1166,.T.);
#2304=EDGE_CURVE('',#1931,#1915,#1167,.T.);
#2305=EDGE_CURVE('',#1926,#1931,#1168,.T.);
#2306=EDGE_CURVE('',#1932,#1927,#1169,.T.);
#2307=EDGE_CURVE('',#1932,#1924,#1170,.T.);
#2308=EDGE_CURVE('',#1933,#1932,#1171,.T.);
#2309=EDGE_CURVE('',#1933,#1923,#1172,.T.);
#2310=EDGE_CURVE('',#1934,#1933,#1173,.T.);
#2311=EDGE_CURVE('',#1934,#1922,#1174,.T.);
#2312=EDGE_CURVE('',#1935,#1934,#1175,.T.);
#2313=EDGE_CURVE('',#1935,#1921,#1176,.T.);
#2314=EDGE_CURVE('',#1936,#1935,#1177,.T.);
#2315=EDGE_CURVE('',#1936,#1920,#1178,.T.);
#2316=EDGE_CURVE('',#1937,#1936,#1179,.T.);
#2317=EDGE_CURVE('',#1937,#1919,#1180,.T.);
#2318=EDGE_CURVE('',#1929,#1937,#1181,.T.);
#2319=EDGE_CURVE('',#1938,#1939,#1182,.T.);
#2320=EDGE_CURVE('',#1938,#1939,#1696,.T.);
#2321=EDGE_CURVE('',#1940,#1940,#1697,.T.);
#2322=EDGE_CURVE('',#1941,#1938,#1183,.T.);
#2323=EDGE_CURVE('',#1942,#1941,#1698,.T.);
#2324=EDGE_CURVE('',#1939,#1942,#1184,.T.);
#2325=EDGE_CURVE('',#1943,#1944,#1185,.T.);
#2326=EDGE_CURVE('',#1943,#1944,#1699,.T.);
#2327=EDGE_CURVE('',#1945,#1945,#1700,.T.);
#2328=EDGE_CURVE('',#1946,#1943,#1186,.T.);
#2329=EDGE_CURVE('',#1947,#1946,#1701,.T.);
#2330=EDGE_CURVE('',#1944,#1947,#1187,.T.);
#2331=EDGE_CURVE('',#1948,#1942,#1188,.T.);
#2332=EDGE_CURVE('',#1949,#1948,#1189,.T.);
#2333=EDGE_CURVE('',#1949,#1950,#1190,.T.);
#2334=EDGE_CURVE('',#1950,#1951,#1191,.T.);
#2335=EDGE_CURVE('',#1941,#1951,#1192,.T.);
#2336=EDGE_CURVE('',#1952,#1947,#1193,.T.);
#2337=EDGE_CURVE('',#1953,#1952,#1194,.T.);
#2338=EDGE_CURVE('',#1953,#1954,#1195,.T.);
#2339=EDGE_CURVE('',#1954,#1955,#1196,.T.);
#2340=EDGE_CURVE('',#1946,#1955,#1197,.T.);
#2341=EDGE_CURVE('',#1956,#1956,#1702,.T.);
#2342=EDGE_CURVE('',#1956,#1940,#1198,.T.);
#2343=EDGE_CURVE('',#1957,#1957,#1703,.T.);
#2344=EDGE_CURVE('',#1957,#1945,#1199,.T.);
#2345=EDGE_CURVE('',#1958,#1959,#1704,.T.);
#2346=EDGE_CURVE('',#1960,#1958,#1200,.T.);
#2347=EDGE_CURVE('',#1961,#1960,#1705,.T.);
#2348=EDGE_CURVE('',#1959,#1961,#1201,.T.);
#2349=EDGE_CURVE('',#1960,#1953,#1202,.T.);
#2350=EDGE_CURVE('',#1951,#1952,#1203,.T.);
#2351=EDGE_CURVE('',#1950,#1961,#1204,.T.);
#2352=EDGE_CURVE('',#1954,#1958,#1205,.T.);
#2353=EDGE_CURVE('',#1959,#1949,#1206,.T.);
#2354=EDGE_CURVE('',#1955,#1948,#1207,.T.);
#2355=EDGE_CURVE('',#1962,#1962,#1706,.T.);
#2356=EDGE_CURVE('',#1962,#1963,#1208,.T.);
#2357=EDGE_CURVE('',#1963,#1963,#1707,.T.);
#2358=EDGE_CURVE('',#1964,#1964,#1708,.T.);
#2359=EDGE_CURVE('',#1965,#1965,#1709,.T.);
#2360=EDGE_CURVE('',#1965,#1964,#1209,.T.);
#2361=EDGE_CURVE('',#1966,#1966,#1710,.T.);
#2362=EDGE_CURVE('',#1966,#1967,#1210,.T.);
#2363=EDGE_CURVE('',#1967,#1967,#1711,.T.);
#2364=EDGE_CURVE('',#1968,#1968,#1712,.T.);
#2365=EDGE_CURVE('',#1968,#1969,#1211,.T.);
#2366=EDGE_CURVE('',#1969,#1969,#1713,.T.);
#2367=EDGE_CURVE('',#1970,#1970,#1714,.T.);
#2368=EDGE_CURVE('',#1970,#1971,#1212,.T.);
#2369=EDGE_CURVE('',#1971,#1971,#1715,.T.);
#2370=EDGE_CURVE('',#1972,#1972,#1716,.T.);
#2371=EDGE_CURVE('',#1972,#1973,#1213,.T.);
#2372=EDGE_CURVE('',#1973,#1973,#1717,.T.);
#2373=EDGE_CURVE('',#1974,#1974,#1718,.T.);
#2374=EDGE_CURVE('',#1974,#1975,#1214,.T.);
#2375=EDGE_CURVE('',#1975,#1975,#1719,.T.);
#2376=EDGE_CURVE('',#1976,#1976,#1720,.T.);
#2377=EDGE_CURVE('',#1977,#1977,#1721,.T.);
#2378=EDGE_CURVE('',#1978,#1978,#1722,.T.);
#2379=EDGE_CURVE('',#1978,#1976,#1215,.T.);
#2380=EDGE_CURVE('',#1979,#1979,#1723,.T.);
#2381=EDGE_CURVE('',#1979,#1980,#1216,.T.);
#2382=EDGE_CURVE('',#1980,#1980,#1724,.T.);
#2383=EDGE_CURVE('',#1977,#1981,#1217,.T.);
#2384=EDGE_CURVE('',#1981,#1981,#1725,.T.);
#2385=EDGE_CURVE('',#1982,#1982,#1726,.T.);
#2386=EDGE_CURVE('',#1982,#1983,#1218,.T.);
#2387=EDGE_CURVE('',#1983,#1983,#1727,.T.);
#2388=EDGE_CURVE('',#1984,#1984,#1728,.T.);
#2389=EDGE_CURVE('',#1984,#1985,#1219,.T.);
#2390=EDGE_CURVE('',#1985,#1985,#1729,.T.);
#2391=EDGE_CURVE('',#1986,#1986,#1730,.T.);
#2392=EDGE_CURVE('',#1986,#1987,#1220,.T.);
#2393=EDGE_CURVE('',#1987,#1987,#1731,.T.);
#2394=EDGE_CURVE('',#1988,#1988,#1732,.T.);
#2395=EDGE_CURVE('',#1988,#1989,#1221,.T.);
#2396=EDGE_CURVE('',#1989,#1989,#1733,.T.);
#2397=EDGE_CURVE('',#1990,#1990,#1734,.T.);
#2398=EDGE_CURVE('',#1990,#1991,#1222,.T.);
#2399=EDGE_CURVE('',#1991,#1991,#1735,.T.);
#2400=EDGE_CURVE('',#1992,#1992,#1736,.T.);
#2401=EDGE_CURVE('',#1992,#1993,#1223,.T.);
#2402=EDGE_CURVE('',#1993,#1993,#1737,.T.);
#2403=EDGE_CURVE('',#1994,#1994,#1738,.T.);
#2404=EDGE_CURVE('',#1994,#1995,#1224,.T.);
#2405=EDGE_CURVE('',#1995,#1995,#1739,.T.);
#2406=EDGE_CURVE('',#1996,#1996,#1740,.T.);
#2407=EDGE_CURVE('',#1997,#1997,#1741,.T.);
#2408=EDGE_CURVE('',#1996,#1998,#1225,.T.);
#2409=EDGE_CURVE('',#1998,#1998,#1742,.T.);
#2410=EDGE_CURVE('',#1999,#1999,#1743,.T.);
#2411=EDGE_CURVE('',#1999,#2000,#1226,.T.);
#2412=EDGE_CURVE('',#2000,#2000,#1744,.T.);
#2413=EDGE_CURVE('',#2001,#2001,#1745,.T.);
#2414=EDGE_CURVE('',#2001,#1997,#1227,.T.);
#2415=EDGE_CURVE('',#2002,#2002,#1746,.T.);
#2416=EDGE_CURVE('',#2002,#2003,#1228,.T.);
#2417=EDGE_CURVE('',#2003,#2003,#1747,.T.);
#2418=EDGE_CURVE('',#2004,#2004,#1748,.T.);
#2419=EDGE_CURVE('',#2004,#2005,#1229,.T.);
#2420=EDGE_CURVE('',#2005,#2005,#1749,.T.);
#2421=EDGE_CURVE('',#2006,#2007,#1230,.T.);
#2422=EDGE_CURVE('',#2007,#2008,#1231,.T.);
#2423=EDGE_CURVE('',#2008,#2009,#1232,.T.);
#2424=EDGE_CURVE('',#2006,#2009,#1233,.T.);
#2425=EDGE_CURVE('',#2007,#2010,#1234,.T.);
#2426=EDGE_CURVE('',#2010,#2011,#1235,.T.);
#2427=EDGE_CURVE('',#2011,#2008,#1236,.T.);
#2428=EDGE_CURVE('',#2010,#2012,#1237,.T.);
#2429=EDGE_CURVE('',#2012,#2013,#1238,.T.);
#2430=EDGE_CURVE('',#2013,#2011,#1239,.T.);
#2431=EDGE_CURVE('',#2012,#2014,#1240,.T.);
#2432=EDGE_CURVE('',#2014,#2015,#1241,.T.);
#2433=EDGE_CURVE('',#2015,#2013,#1242,.T.);
#2434=EDGE_CURVE('',#2014,#2016,#1243,.T.);
#2435=EDGE_CURVE('',#2016,#2017,#1244,.T.);
#2436=EDGE_CURVE('',#2017,#2015,#1245,.T.);
#2437=EDGE_CURVE('',#2016,#2006,#1246,.T.);
#2438=EDGE_CURVE('',#2009,#2017,#1247,.T.);
#2439=EDGE_CURVE('',#2018,#2018,#1750,.T.);
#2440=EDGE_CURVE('',#2019,#2019,#1751,.T.);
#2441=EDGE_CURVE('',#2020,#2020,#1752,.T.);
#2442=EDGE_CURVE('',#2020,#2019,#1248,.T.);
#2443=EDGE_CURVE('',#2021,#2021,#1753,.T.);
#2444=EDGE_CURVE('',#2021,#2020,#1249,.T.);
#2445=EDGE_CURVE('',#2022,#2022,#1754,.T.);
#2446=EDGE_CURVE('',#2022,#2021,#1250,.T.);
#2447=EDGE_CURVE('',#2023,#2023,#1755,.T.);
#2448=EDGE_CURVE('',#2024,#2024,#1756,.F.);
#2449=EDGE_CURVE('',#2024,#2023,#1251,.T.);
#2450=EDGE_CURVE('',#2018,#2024,#1252,.T.);
#2451=EDGE_CURVE('',#2025,#2025,#1757,.T.);
#2452=EDGE_CURVE('',#2026,#2026,#1758,.T.);
#2453=EDGE_CURVE('',#2026,#2025,#1253,.T.);
#2454=EDGE_CURVE('',#2027,#2027,#1759,.T.);
#2455=EDGE_CURVE('',#2027,#2026,#1254,.T.);
#2456=EDGE_CURVE('',#2028,#2028,#1760,.T.);
#2457=EDGE_CURVE('',#2028,#2027,#1255,.T.);
#2458=EDGE_CURVE('',#2029,#2029,#1761,.T.);
#2459=EDGE_CURVE('',#2030,#2030,#1762,.F.);
#2460=EDGE_CURVE('',#2030,#2029,#1256,.T.);
#2461=EDGE_CURVE('',#2031,#2031,#1763,.F.);
#2462=EDGE_CURVE('',#2031,#2030,#1257,.T.);
#2463=EDGE_CURVE('',#2032,#2032,#1764,.T.);
#2464=EDGE_CURVE('',#2032,#2031,#1258,.T.);
#2465=EDGE_CURVE('',#2033,#2034,#1259,.T.);
#2466=EDGE_CURVE('',#2034,#2035,#1260,.T.);
#2467=EDGE_CURVE('',#2035,#2036,#1261,.T.);
#2468=EDGE_CURVE('',#2033,#2036,#1262,.T.);
#2469=EDGE_CURVE('',#2034,#2037,#1263,.T.);
#2470=EDGE_CURVE('',#2037,#2038,#1264,.T.);
#2471=EDGE_CURVE('',#2038,#2035,#1265,.T.);
#2472=EDGE_CURVE('',#2037,#2039,#1266,.T.);
#2473=EDGE_CURVE('',#2039,#2040,#1267,.T.);
#2474=EDGE_CURVE('',#2040,#2038,#1268,.T.);
#2475=EDGE_CURVE('',#2039,#2041,#1269,.T.);
#2476=EDGE_CURVE('',#2041,#2042,#1270,.T.);
#2477=EDGE_CURVE('',#2042,#2040,#1271,.T.);
#2478=EDGE_CURVE('',#2041,#2043,#1272,.T.);
#2479=EDGE_CURVE('',#2043,#2044,#1273,.T.);
#2480=EDGE_CURVE('',#2044,#2042,#1274,.T.);
#2481=EDGE_CURVE('',#2043,#2033,#1275,.T.);
#2482=EDGE_CURVE('',#2036,#2044,#1276,.T.);
#2483=EDGE_CURVE('',#2045,#2046,#185,.T.);
#2484=EDGE_CURVE('',#2047,#2045,#1765,.T.);
#2485=EDGE_CURVE('',#2047,#2048,#1277,.T.);
#2486=EDGE_CURVE('',#2048,#2048,#1766,.T.);
#2487=EDGE_CURVE('',#2046,#2047,#1767,.T.);
#2488=EDGE_CURVE('',#2049,#2050,#1768,.T.);
#2489=EDGE_CURVE('',#2045,#2051,#1769,.T.);
#2490=EDGE_CURVE('',#2051,#2046,#1770,.T.);
#2491=EDGE_CURVE('',#2051,#2052,#1278,.T.);
#2492=EDGE_CURVE('',#2052,#2052,#1771,.T.);
#2493=EDGE_CURVE('',#2053,#2053,#1772,.T.);
#2494=EDGE_CURVE('',#2054,#2054,#1773,.T.);
#2495=EDGE_CURVE('',#2054,#2053,#1279,.T.);
#2496=EDGE_CURVE('',#2055,#2055,#1774,.T.);
#2497=EDGE_CURVE('',#2055,#2056,#1280,.T.);
#2498=EDGE_CURVE('',#2056,#2056,#1775,.T.);
#2499=EDGE_CURVE('',#2057,#2058,#1776,.T.);
#2500=EDGE_CURVE('',#2058,#2059,#1777,.T.);
#2501=EDGE_CURVE('',#2060,#2059,#1778,.T.);
#2502=EDGE_CURVE('',#2057,#2060,#1779,.T.);
#2503=EDGE_CURVE('',#2059,#2057,#186,.T.);
#2504=EDGE_CURVE('',#2058,#2061,#1281,.T.);
#2505=EDGE_CURVE('',#2061,#2061,#1780,.T.);
#2506=EDGE_CURVE('',#2062,#2062,#1781,.T.);
#2507=EDGE_CURVE('',#2063,#2063,#1782,.T.);
#2508=EDGE_CURVE('',#2063,#2062,#1282,.T.);
#2509=EDGE_CURVE('',#2064,#2064,#1783,.T.);
#2510=EDGE_CURVE('',#2065,#2065,#1784,.T.);
#2511=EDGE_CURVE('',#2066,#2066,#1785,.T.);
#2512=EDGE_CURVE('',#2066,#2064,#1283,.T.);
#2513=EDGE_CURVE('',#2065,#2060,#1284,.T.);
#2514=EDGE_CURVE('',#2067,#2068,#1285,.T.);
#2515=EDGE_CURVE('',#2068,#2069,#1286,.T.);
#2516=EDGE_CURVE('',#2069,#2070,#1287,.T.);
#2517=EDGE_CURVE('',#2070,#2071,#1288,.T.);
#2518=EDGE_CURVE('',#2071,#2072,#1289,.T.);
#2519=EDGE_CURVE('',#2072,#2067,#1290,.T.);
#2520=EDGE_CURVE('',#2073,#2073,#1786,.T.);
#2521=EDGE_CURVE('',#2074,#2075,#1291,.T.);
#2522=EDGE_CURVE('',#2075,#2076,#1292,.T.);
#2523=EDGE_CURVE('',#2076,#2077,#1293,.T.);
#2524=EDGE_CURVE('',#2077,#2078,#1294,.T.);
#2525=EDGE_CURVE('',#2078,#2079,#1295,.T.);
#2526=EDGE_CURVE('',#2079,#2074,#1296,.T.);
#2527=EDGE_CURVE('',#2080,#2080,#1787,.T.);
#2528=EDGE_CURVE('',#2074,#2068,#1297,.T.);
#2529=EDGE_CURVE('',#2069,#2079,#1298,.T.);
#2530=EDGE_CURVE('',#2070,#2078,#1299,.T.);
#2531=EDGE_CURVE('',#2071,#2077,#1300,.T.);
#2532=EDGE_CURVE('',#2072,#2076,#1301,.T.);
#2533=EDGE_CURVE('',#2067,#2075,#1302,.T.);
#2534=EDGE_CURVE('',#2080,#2081,#1303,.T.);
#2535=EDGE_CURVE('',#2081,#2081,#1788,.T.);
#2536=EDGE_CURVE('',#2082,#2082,#1789,.T.);
#2537=EDGE_CURVE('',#2083,#2083,#1790,.T.);
#2538=EDGE_CURVE('',#2081,#2082,#1304,.T.);
#2539=EDGE_CURVE('',#2084,#2084,#1791,.T.);
#2540=EDGE_CURVE('',#2084,#2073,#1305,.T.);
#2541=EDGE_CURVE('',#2085,#2085,#1792,.T.);
#2542=EDGE_CURVE('',#2085,#2084,#1306,.T.);
#2543=EDGE_CURVE('',#2086,#2086,#1793,.T.);
#2544=EDGE_CURVE('',#2086,#2083,#1307,.T.);
#2545=EDGE_CURVE('',#2087,#2087,#1794,.T.);
#2546=EDGE_CURVE('',#2088,#2088,#1795,.T.);
#2547=EDGE_CURVE('',#2088,#2087,#1308,.T.);
#2548=EDGE_CURVE('',#2089,#2089,#1796,.T.);
#2549=EDGE_CURVE('',#2089,#2088,#1309,.T.);
#2550=EDGE_CURVE('',#2090,#2090,#1797,.T.);
#2551=EDGE_CURVE('',#2090,#2089,#1310,.T.);
#2552=EDGE_CURVE('',#2091,#2091,#1798,.T.);
#2553=EDGE_CURVE('',#2092,#2092,#1799,.F.);
#2554=EDGE_CURVE('',#2092,#2091,#1311,.T.);
#2555=EDGE_CURVE('',#2093,#2093,#1800,.F.);
#2556=EDGE_CURVE('',#2093,#2092,#1312,.T.);
#2557=EDGE_CURVE('',#2094,#2094,#1801,.T.);
#2558=EDGE_CURVE('',#2094,#2093,#1313,.T.);
#2559=EDGE_CURVE('',#2095,#2096,#1314,.T.);
#2560=EDGE_CURVE('',#2096,#2097,#1315,.T.);
#2561=EDGE_CURVE('',#2097,#2098,#1316,.T.);
#2562=EDGE_CURVE('',#2095,#2098,#1317,.T.);
#2563=EDGE_CURVE('',#2096,#2099,#1318,.T.);
#2564=EDGE_CURVE('',#2099,#2100,#1319,.T.);
#2565=EDGE_CURVE('',#2100,#2097,#1320,.T.);
#2566=EDGE_CURVE('',#2099,#2101,#1321,.T.);
#2567=EDGE_CURVE('',#2101,#2102,#1322,.T.);
#2568=EDGE_CURVE('',#2102,#2100,#1323,.T.);
#2569=EDGE_CURVE('',#2101,#2103,#1324,.T.);
#2570=EDGE_CURVE('',#2103,#2104,#1325,.T.);
#2571=EDGE_CURVE('',#2104,#2102,#1326,.T.);
#2572=EDGE_CURVE('',#2103,#2105,#1327,.T.);
#2573=EDGE_CURVE('',#2105,#2106,#1328,.T.);
#2574=EDGE_CURVE('',#2106,#2104,#1329,.T.);
#2575=EDGE_CURVE('',#2105,#2095,#1330,.T.);
#2576=EDGE_CURVE('',#2098,#2106,#1331,.T.);
#2577=EDGE_CURVE('',#2107,#2107,#1802,.T.);
#2578=EDGE_CURVE('',#2107,#2108,#1332,.T.);
#2579=EDGE_CURVE('',#2108,#2108,#1803,.T.);
#2580=EDGE_CURVE('',#2109,#2109,#1804,.T.);
#2581=EDGE_CURVE('',#2109,#2110,#1333,.T.);
#2582=EDGE_CURVE('',#2110,#2110,#1805,.T.);
#2583=EDGE_CURVE('',#2111,#2112,#171,.T.);
#2584=EDGE_CURVE('',#2113,#2111,#172,.T.);
#2585=EDGE_CURVE('',#2113,#2114,#1334,.T.);
#2586=EDGE_CURVE('',#2114,#2114,#1806,.T.);
#2587=EDGE_CURVE('',#2115,#2113,#173,.T.);
#2588=EDGE_CURVE('',#2116,#2115,#174,.T.);
#2589=EDGE_CURVE('',#2117,#2116,#175,.T.);
#2590=EDGE_CURVE('',#2112,#2117,#176,.T.);
#2591=EDGE_CURVE('',#2118,#2118,#1807,.T.);
#2592=EDGE_CURVE('',#2118,#2119,#1335,.T.);
#2593=EDGE_CURVE('',#2120,#2119,#177,.T.);
#2594=EDGE_CURVE('',#2121,#2120,#178,.T.);
#2595=EDGE_CURVE('',#2122,#2121,#179,.T.);
#2596=EDGE_CURVE('',#2123,#2122,#180,.T.);
#2597=EDGE_CURVE('',#2124,#2123,#181,.T.);
#2598=EDGE_CURVE('',#2119,#2124,#182,.T.);
#2599=EDGE_CURVE('',#2115,#2124,#1336,.T.);
#2600=EDGE_CURVE('',#2116,#2123,#1337,.T.);
#2601=EDGE_CURVE('',#2113,#2119,#1338,.T.);
#2602=EDGE_CURVE('',#2111,#2120,#1339,.T.);
#2603=EDGE_CURVE('',#2125,#2125,#1808,.F.);
#2604=EDGE_CURVE('',#2125,#2126,#1340,.T.);
#2605=EDGE_CURVE('',#2126,#2126,#1809,.F.);
#2606=EDGE_CURVE('',#2112,#2121,#1341,.T.);
#2607=EDGE_CURVE('',#2117,#2122,#1342,.T.);
#2608=ORIENTED_EDGE('',*,*,#2127,.F.);
#2609=ORIENTED_EDGE('',*,*,#2128,.T.);
#2610=ORIENTED_EDGE('',*,*,#2129,.F.);
#2611=ORIENTED_EDGE('',*,*,#2128,.F.);
#2612=ORIENTED_EDGE('',*,*,#2130,.F.);
#2613=ORIENTED_EDGE('',*,*,#2131,.T.);
#2614=ORIENTED_EDGE('',*,*,#2132,.F.);
#2615=ORIENTED_EDGE('',*,*,#2131,.F.);
#2616=ORIENTED_EDGE('',*,*,#2133,.F.);
#2617=ORIENTED_EDGE('',*,*,#2134,.T.);
#2618=ORIENTED_EDGE('',*,*,#2135,.F.);
#2619=ORIENTED_EDGE('',*,*,#2134,.F.);
#2620=ORIENTED_EDGE('',*,*,#2136,.F.);
#2621=ORIENTED_EDGE('',*,*,#2137,.T.);
#2622=ORIENTED_EDGE('',*,*,#2138,.F.);
#2623=ORIENTED_EDGE('',*,*,#2137,.F.);
#2624=ORIENTED_EDGE('',*,*,#2139,.T.);
#2625=ORIENTED_EDGE('',*,*,#2140,.T.);
#2626=ORIENTED_EDGE('',*,*,#2141,.F.);
#2627=ORIENTED_EDGE('',*,*,#2142,.F.);
#2628=ORIENTED_EDGE('',*,*,#2143,.T.);
#2629=ORIENTED_EDGE('',*,*,#2142,.T.);
#2630=ORIENTED_EDGE('',*,*,#2144,.F.);
#2631=ORIENTED_EDGE('',*,*,#2145,.F.);
#2632=ORIENTED_EDGE('',*,*,#2146,.T.);
#2633=ORIENTED_EDGE('',*,*,#2145,.T.);
#2634=ORIENTED_EDGE('',*,*,#2147,.F.);
#2635=ORIENTED_EDGE('',*,*,#2148,.F.);
#2636=ORIENTED_EDGE('',*,*,#2149,.T.);
#2637=ORIENTED_EDGE('',*,*,#2148,.T.);
#2638=ORIENTED_EDGE('',*,*,#2150,.F.);
#2639=ORIENTED_EDGE('',*,*,#2140,.F.);
#2640=ORIENTED_EDGE('',*,*,#2150,.T.);
#2641=ORIENTED_EDGE('',*,*,#2147,.T.);
#2642=ORIENTED_EDGE('',*,*,#2144,.T.);
#2643=ORIENTED_EDGE('',*,*,#2141,.T.);
#2644=ORIENTED_EDGE('',*,*,#2129,.T.);
#2645=ORIENTED_EDGE('',*,*,#2132,.T.);
#2646=ORIENTED_EDGE('',*,*,#2135,.T.);
#2647=ORIENTED_EDGE('',*,*,#2138,.T.);
#2648=ORIENTED_EDGE('',*,*,#2149,.F.);
#2649=ORIENTED_EDGE('',*,*,#2139,.F.);
#2650=ORIENTED_EDGE('',*,*,#2143,.F.);
#2651=ORIENTED_EDGE('',*,*,#2146,.F.);
#2652=ORIENTED_EDGE('',*,*,#2127,.T.);
#2653=ORIENTED_EDGE('',*,*,#2130,.T.);
#2654=ORIENTED_EDGE('',*,*,#2133,.T.);
#2655=ORIENTED_EDGE('',*,*,#2136,.T.);
#2656=ORIENTED_EDGE('',*,*,#2151,.T.);
#2657=ORIENTED_EDGE('',*,*,#2152,.T.);
#2658=ORIENTED_EDGE('',*,*,#2153,.F.);
#2659=ORIENTED_EDGE('',*,*,#2154,.F.);
#2660=ORIENTED_EDGE('',*,*,#2155,.T.);
#2661=ORIENTED_EDGE('',*,*,#2154,.T.);
#2662=ORIENTED_EDGE('',*,*,#2156,.F.);
#2663=ORIENTED_EDGE('',*,*,#2157,.F.);
#2664=ORIENTED_EDGE('',*,*,#2158,.T.);
#2665=ORIENTED_EDGE('',*,*,#2157,.T.);
#2666=ORIENTED_EDGE('',*,*,#2159,.F.);
#2667=ORIENTED_EDGE('',*,*,#2160,.F.);
#2668=ORIENTED_EDGE('',*,*,#2161,.T.);
#2669=ORIENTED_EDGE('',*,*,#2160,.T.);
#2670=ORIENTED_EDGE('',*,*,#2162,.F.);
#2671=ORIENTED_EDGE('',*,*,#2152,.F.);
#2672=ORIENTED_EDGE('',*,*,#2162,.T.);
#2673=ORIENTED_EDGE('',*,*,#2159,.T.);
#2674=ORIENTED_EDGE('',*,*,#2156,.T.);
#2675=ORIENTED_EDGE('',*,*,#2153,.T.);
#2676=ORIENTED_EDGE('',*,*,#2161,.F.);
#2677=ORIENTED_EDGE('',*,*,#2151,.F.);
#2678=ORIENTED_EDGE('',*,*,#2155,.F.);
#2679=ORIENTED_EDGE('',*,*,#2158,.F.);
#2680=ORIENTED_EDGE('',*,*,#2163,.T.);
#2681=ORIENTED_EDGE('',*,*,#2164,.T.);
#2682=ORIENTED_EDGE('',*,*,#2165,.F.);
#2683=ORIENTED_EDGE('',*,*,#2166,.F.);
#2684=ORIENTED_EDGE('',*,*,#2167,.T.);
#2685=ORIENTED_EDGE('',*,*,#2166,.T.);
#2686=ORIENTED_EDGE('',*,*,#2168,.F.);
#2687=ORIENTED_EDGE('',*,*,#2169,.F.);
#2688=ORIENTED_EDGE('',*,*,#2170,.T.);
#2689=ORIENTED_EDGE('',*,*,#2169,.T.);
#2690=ORIENTED_EDGE('',*,*,#2171,.F.);
#2691=ORIENTED_EDGE('',*,*,#2172,.F.);
#2692=ORIENTED_EDGE('',*,*,#2173,.T.);
#2693=ORIENTED_EDGE('',*,*,#2172,.T.);
#2694=ORIENTED_EDGE('',*,*,#2174,.F.);
#2695=ORIENTED_EDGE('',*,*,#2164,.F.);
#2696=ORIENTED_EDGE('',*,*,#2174,.T.);
#2697=ORIENTED_EDGE('',*,*,#2171,.T.);
#2698=ORIENTED_EDGE('',*,*,#2168,.T.);
#2699=ORIENTED_EDGE('',*,*,#2165,.T.);
#2700=ORIENTED_EDGE('',*,*,#2173,.F.);
#2701=ORIENTED_EDGE('',*,*,#2163,.F.);
#2702=ORIENTED_EDGE('',*,*,#2167,.F.);
#2703=ORIENTED_EDGE('',*,*,#2170,.F.);
#2704=ORIENTED_EDGE('',*,*,#2175,.F.);
#2705=ORIENTED_EDGE('',*,*,#2176,.T.);
#2706=ORIENTED_EDGE('',*,*,#2177,.F.);
#2707=ORIENTED_EDGE('',*,*,#2176,.F.);
#2708=ORIENTED_EDGE('',*,*,#2175,.T.);
#2709=ORIENTED_EDGE('',*,*,#2178,.F.);
#2710=ORIENTED_EDGE('',*,*,#2179,.T.);
#2711=ORIENTED_EDGE('',*,*,#2180,.F.);
#2712=ORIENTED_EDGE('',*,*,#2179,.F.);
#2713=ORIENTED_EDGE('',*,*,#2178,.T.);
#2714=ORIENTED_EDGE('',*,*,#2181,.F.);
#2715=ORIENTED_EDGE('',*,*,#2182,.T.);
#2716=ORIENTED_EDGE('',*,*,#2183,.F.);
#2717=ORIENTED_EDGE('',*,*,#2182,.F.);
#2718=ORIENTED_EDGE('',*,*,#2184,.F.);
#2719=ORIENTED_EDGE('',*,*,#2185,.T.);
#2720=ORIENTED_EDGE('',*,*,#2186,.F.);
#2721=ORIENTED_EDGE('',*,*,#2185,.F.);
#2722=ORIENTED_EDGE('',*,*,#2187,.F.);
#2723=ORIENTED_EDGE('',*,*,#2188,.F.);
#2724=ORIENTED_EDGE('',*,*,#2189,.F.);
#2725=ORIENTED_EDGE('',*,*,#2190,.F.);
#2726=ORIENTED_EDGE('',*,*,#2188,.T.);
#2727=ORIENTED_EDGE('',*,*,#2191,.T.);
#2728=ORIENTED_EDGE('',*,*,#2192,.T.);
#2729=ORIENTED_EDGE('',*,*,#2193,.T.);
#2730=ORIENTED_EDGE('',*,*,#2194,.T.);
#2731=ORIENTED_EDGE('',*,*,#2195,.T.);
#2732=ORIENTED_EDGE('',*,*,#2196,.T.);
#2733=ORIENTED_EDGE('',*,*,#2197,.T.);
#2734=ORIENTED_EDGE('',*,*,#2198,.T.);
#2735=ORIENTED_EDGE('',*,*,#2199,.T.);
#2736=ORIENTED_EDGE('',*,*,#2200,.T.);
#2737=ORIENTED_EDGE('',*,*,#2201,.T.);
#2738=ORIENTED_EDGE('',*,*,#2202,.T.);
#2739=ORIENTED_EDGE('',*,*,#2203,.T.);
#2740=ORIENTED_EDGE('',*,*,#2187,.T.);
#2741=ORIENTED_EDGE('',*,*,#2204,.T.);
#2742=ORIENTED_EDGE('',*,*,#2205,.T.);
#2743=ORIENTED_EDGE('',*,*,#2191,.F.);
#2744=ORIENTED_EDGE('',*,*,#2177,.T.);
#2745=ORIENTED_EDGE('',*,*,#2189,.T.);
#2746=ORIENTED_EDGE('',*,*,#2203,.F.);
#2747=ORIENTED_EDGE('',*,*,#2206,.F.);
#2748=ORIENTED_EDGE('',*,*,#2207,.T.);
#2749=ORIENTED_EDGE('',*,*,#2180,.T.);
#2750=ORIENTED_EDGE('',*,*,#2208,.T.);
#2751=ORIENTED_EDGE('',*,*,#2209,.T.);
#2752=ORIENTED_EDGE('',*,*,#2195,.F.);
#2753=ORIENTED_EDGE('',*,*,#2210,.F.);
#2754=ORIENTED_EDGE('',*,*,#2183,.T.);
#2755=ORIENTED_EDGE('',*,*,#2211,.T.);
#2756=ORIENTED_EDGE('',*,*,#2210,.T.);
#2757=ORIENTED_EDGE('',*,*,#2194,.F.);
#2758=ORIENTED_EDGE('',*,*,#2212,.F.);
#2759=ORIENTED_EDGE('',*,*,#2213,.T.);
#2760=ORIENTED_EDGE('',*,*,#2212,.T.);
#2761=ORIENTED_EDGE('',*,*,#2193,.F.);
#2762=ORIENTED_EDGE('',*,*,#2214,.F.);
#2763=ORIENTED_EDGE('',*,*,#2215,.T.);
#2764=ORIENTED_EDGE('',*,*,#2214,.T.);
#2765=ORIENTED_EDGE('',*,*,#2192,.F.);
#2766=ORIENTED_EDGE('',*,*,#2205,.F.);
#2767=ORIENTED_EDGE('',*,*,#2216,.T.);
#2768=ORIENTED_EDGE('',*,*,#2206,.T.);
#2769=ORIENTED_EDGE('',*,*,#2202,.F.);
#2770=ORIENTED_EDGE('',*,*,#2217,.F.);
#2771=ORIENTED_EDGE('',*,*,#2218,.T.);
#2772=ORIENTED_EDGE('',*,*,#2217,.T.);
#2773=ORIENTED_EDGE('',*,*,#2201,.F.);
#2774=ORIENTED_EDGE('',*,*,#2219,.F.);
#2775=ORIENTED_EDGE('',*,*,#2220,.T.);
#2776=ORIENTED_EDGE('',*,*,#2219,.T.);
#2777=ORIENTED_EDGE('',*,*,#2200,.F.);
#2778=ORIENTED_EDGE('',*,*,#2221,.F.);
#2779=ORIENTED_EDGE('',*,*,#2222,.T.);
#2780=ORIENTED_EDGE('',*,*,#2221,.T.);
#2781=ORIENTED_EDGE('',*,*,#2199,.F.);
#2782=ORIENTED_EDGE('',*,*,#2223,.F.);
#2783=ORIENTED_EDGE('',*,*,#2186,.T.);
#2784=ORIENTED_EDGE('',*,*,#2224,.T.);
#2785=ORIENTED_EDGE('',*,*,#2223,.T.);
#2786=ORIENTED_EDGE('',*,*,#2198,.F.);
#2787=ORIENTED_EDGE('',*,*,#2225,.F.);
#2788=ORIENTED_EDGE('',*,*,#2226,.T.);
#2789=ORIENTED_EDGE('',*,*,#2225,.T.);
#2790=ORIENTED_EDGE('',*,*,#2197,.F.);
#2791=ORIENTED_EDGE('',*,*,#2227,.F.);
#2792=ORIENTED_EDGE('',*,*,#2181,.T.);
#2793=ORIENTED_EDGE('',*,*,#2184,.T.);
#2794=ORIENTED_EDGE('',*,*,#2228,.T.);
#2795=ORIENTED_EDGE('',*,*,#2227,.T.);
#2796=ORIENTED_EDGE('',*,*,#2196,.F.);
#2797=ORIENTED_EDGE('',*,*,#2209,.F.);
#2798=ORIENTED_EDGE('',*,*,#2190,.T.);
#2799=ORIENTED_EDGE('',*,*,#2207,.F.);
#2800=ORIENTED_EDGE('',*,*,#2216,.F.);
#2801=ORIENTED_EDGE('',*,*,#2218,.F.);
#2802=ORIENTED_EDGE('',*,*,#2220,.F.);
#2803=ORIENTED_EDGE('',*,*,#2222,.F.);
#2804=ORIENTED_EDGE('',*,*,#2224,.F.);
#2805=ORIENTED_EDGE('',*,*,#2226,.F.);
#2806=ORIENTED_EDGE('',*,*,#2228,.F.);
#2807=ORIENTED_EDGE('',*,*,#2208,.F.);
#2808=ORIENTED_EDGE('',*,*,#2211,.F.);
#2809=ORIENTED_EDGE('',*,*,#2213,.F.);
#2810=ORIENTED_EDGE('',*,*,#2215,.F.);
#2811=ORIENTED_EDGE('',*,*,#2204,.F.);
#2812=ORIENTED_EDGE('',*,*,#2229,.F.);
#2813=ORIENTED_EDGE('',*,*,#2230,.T.);
#2814=ORIENTED_EDGE('',*,*,#2231,.F.);
#2815=ORIENTED_EDGE('',*,*,#2232,.F.);
#2816=ORIENTED_EDGE('',*,*,#2233,.F.);
#2817=ORIENTED_EDGE('',*,*,#2234,.F.);
#2818=ORIENTED_EDGE('',*,*,#2230,.F.);
#2819=ORIENTED_EDGE('',*,*,#2235,.F.);
#2820=ORIENTED_EDGE('',*,*,#2236,.T.);
#2821=ORIENTED_EDGE('',*,*,#2237,.F.);
#2822=ORIENTED_EDGE('',*,*,#2238,.F.);
#2823=ORIENTED_EDGE('',*,*,#2239,.F.);
#2824=ORIENTED_EDGE('',*,*,#2240,.F.);
#2825=ORIENTED_EDGE('',*,*,#2236,.F.);
#2826=ORIENTED_EDGE('',*,*,#2232,.T.);
#2827=ORIENTED_EDGE('',*,*,#2229,.T.);
#2828=ORIENTED_EDGE('',*,*,#2234,.T.);
#2829=ORIENTED_EDGE('',*,*,#2241,.F.);
#2830=ORIENTED_EDGE('',*,*,#2242,.F.);
#2831=ORIENTED_EDGE('',*,*,#2243,.T.);
#2832=ORIENTED_EDGE('',*,*,#2244,.T.);
#2833=ORIENTED_EDGE('',*,*,#2245,.F.);
#2834=ORIENTED_EDGE('',*,*,#2238,.T.);
#2835=ORIENTED_EDGE('',*,*,#2235,.T.);
#2836=ORIENTED_EDGE('',*,*,#2240,.T.);
#2837=ORIENTED_EDGE('',*,*,#2246,.F.);
#2838=ORIENTED_EDGE('',*,*,#2247,.F.);
#2839=ORIENTED_EDGE('',*,*,#2248,.T.);
#2840=ORIENTED_EDGE('',*,*,#2249,.T.);
#2841=ORIENTED_EDGE('',*,*,#2250,.F.);
#2842=ORIENTED_EDGE('',*,*,#2251,.F.);
#2843=ORIENTED_EDGE('',*,*,#2252,.T.);
#2844=ORIENTED_EDGE('',*,*,#2231,.T.);
#2845=ORIENTED_EDGE('',*,*,#2252,.F.);
#2846=ORIENTED_EDGE('',*,*,#2253,.F.);
#2847=ORIENTED_EDGE('',*,*,#2254,.T.);
#2848=ORIENTED_EDGE('',*,*,#2237,.T.);
#2849=ORIENTED_EDGE('',*,*,#2254,.F.);
#2850=ORIENTED_EDGE('',*,*,#2255,.F.);
#2851=ORIENTED_EDGE('',*,*,#2256,.F.);
#2852=ORIENTED_EDGE('',*,*,#2257,.F.);
#2853=ORIENTED_EDGE('',*,*,#2258,.F.);
#2854=ORIENTED_EDGE('',*,*,#2257,.T.);
#2855=ORIENTED_EDGE('',*,*,#2259,.T.);
#2856=ORIENTED_EDGE('',*,*,#2247,.T.);
#2857=ORIENTED_EDGE('',*,*,#2260,.F.);
#2858=ORIENTED_EDGE('',*,*,#2244,.F.);
#2859=ORIENTED_EDGE('',*,*,#2261,.T.);
#2860=ORIENTED_EDGE('',*,*,#2256,.T.);
#2861=ORIENTED_EDGE('',*,*,#2262,.F.);
#2862=ORIENTED_EDGE('',*,*,#2248,.F.);
#2863=ORIENTED_EDGE('',*,*,#2259,.F.);
#2864=ORIENTED_EDGE('',*,*,#2253,.T.);
#2865=ORIENTED_EDGE('',*,*,#2255,.T.);
#2866=ORIENTED_EDGE('',*,*,#2263,.T.);
#2867=ORIENTED_EDGE('',*,*,#2242,.T.);
#2868=ORIENTED_EDGE('',*,*,#2264,.F.);
#2869=ORIENTED_EDGE('',*,*,#2249,.F.);
#2870=ORIENTED_EDGE('',*,*,#2262,.T.);
#2871=ORIENTED_EDGE('',*,*,#2233,.T.);
#2872=ORIENTED_EDGE('',*,*,#2245,.T.);
#2873=ORIENTED_EDGE('',*,*,#2260,.T.);
#2874=ORIENTED_EDGE('',*,*,#2246,.T.);
#2875=ORIENTED_EDGE('',*,*,#2239,.T.);
#2876=ORIENTED_EDGE('',*,*,#2250,.T.);
#2877=ORIENTED_EDGE('',*,*,#2264,.T.);
#2878=ORIENTED_EDGE('',*,*,#2241,.T.);
#2879=ORIENTED_EDGE('',*,*,#2258,.T.);
#2880=ORIENTED_EDGE('',*,*,#2261,.F.);
#2881=ORIENTED_EDGE('',*,*,#2243,.F.);
#2882=ORIENTED_EDGE('',*,*,#2263,.F.);
#2883=ORIENTED_EDGE('',*,*,#2251,.T.);
#2884=ORIENTED_EDGE('',*,*,#2265,.F.);
#2885=ORIENTED_EDGE('',*,*,#2266,.T.);
#2886=ORIENTED_EDGE('',*,*,#2267,.F.);
#2887=ORIENTED_EDGE('',*,*,#2266,.F.);
#2888=ORIENTED_EDGE('',*,*,#2265,.T.);
#2889=ORIENTED_EDGE('',*,*,#2268,.F.);
#2890=ORIENTED_EDGE('',*,*,#2269,.T.);
#2891=ORIENTED_EDGE('',*,*,#2270,.F.);
#2892=ORIENTED_EDGE('',*,*,#2269,.F.);
#2893=ORIENTED_EDGE('',*,*,#2268,.T.);
#2894=ORIENTED_EDGE('',*,*,#2271,.F.);
#2895=ORIENTED_EDGE('',*,*,#2272,.T.);
#2896=ORIENTED_EDGE('',*,*,#2273,.F.);
#2897=ORIENTED_EDGE('',*,*,#2272,.F.);
#2898=ORIENTED_EDGE('',*,*,#2274,.F.);
#2899=ORIENTED_EDGE('',*,*,#2275,.T.);
#2900=ORIENTED_EDGE('',*,*,#2276,.F.);
#2901=ORIENTED_EDGE('',*,*,#2275,.F.);
#2902=ORIENTED_EDGE('',*,*,#2277,.F.);
#2903=ORIENTED_EDGE('',*,*,#2278,.F.);
#2904=ORIENTED_EDGE('',*,*,#2279,.F.);
#2905=ORIENTED_EDGE('',*,*,#2280,.F.);
#2906=ORIENTED_EDGE('',*,*,#2278,.T.);
#2907=ORIENTED_EDGE('',*,*,#2281,.T.);
#2908=ORIENTED_EDGE('',*,*,#2282,.T.);
#2909=ORIENTED_EDGE('',*,*,#2283,.T.);
#2910=ORIENTED_EDGE('',*,*,#2284,.T.);
#2911=ORIENTED_EDGE('',*,*,#2285,.T.);
#2912=ORIENTED_EDGE('',*,*,#2286,.T.);
#2913=ORIENTED_EDGE('',*,*,#2287,.T.);
#2914=ORIENTED_EDGE('',*,*,#2288,.T.);
#2915=ORIENTED_EDGE('',*,*,#2289,.T.);
#2916=ORIENTED_EDGE('',*,*,#2290,.T.);
#2917=ORIENTED_EDGE('',*,*,#2291,.T.);
#2918=ORIENTED_EDGE('',*,*,#2292,.T.);
#2919=ORIENTED_EDGE('',*,*,#2293,.T.);
#2920=ORIENTED_EDGE('',*,*,#2277,.T.);
#2921=ORIENTED_EDGE('',*,*,#2294,.T.);
#2922=ORIENTED_EDGE('',*,*,#2295,.T.);
#2923=ORIENTED_EDGE('',*,*,#2281,.F.);
#2924=ORIENTED_EDGE('',*,*,#2267,.T.);
#2925=ORIENTED_EDGE('',*,*,#2279,.T.);
#2926=ORIENTED_EDGE('',*,*,#2293,.F.);
#2927=ORIENTED_EDGE('',*,*,#2296,.F.);
#2928=ORIENTED_EDGE('',*,*,#2297,.T.);
#2929=ORIENTED_EDGE('',*,*,#2270,.T.);
#2930=ORIENTED_EDGE('',*,*,#2298,.T.);
#2931=ORIENTED_EDGE('',*,*,#2299,.T.);
#2932=ORIENTED_EDGE('',*,*,#2285,.F.);
#2933=ORIENTED_EDGE('',*,*,#2300,.F.);
#2934=ORIENTED_EDGE('',*,*,#2273,.T.);
#2935=ORIENTED_EDGE('',*,*,#2301,.T.);
#2936=ORIENTED_EDGE('',*,*,#2300,.T.);
#2937=ORIENTED_EDGE('',*,*,#2284,.F.);
#2938=ORIENTED_EDGE('',*,*,#2302,.F.);
#2939=ORIENTED_EDGE('',*,*,#2303,.T.);
#2940=ORIENTED_EDGE('',*,*,#2302,.T.);
#2941=ORIENTED_EDGE('',*,*,#2283,.F.);
#2942=ORIENTED_EDGE('',*,*,#2304,.F.);
#2943=ORIENTED_EDGE('',*,*,#2305,.T.);
#2944=ORIENTED_EDGE('',*,*,#2304,.T.);
#2945=ORIENTED_EDGE('',*,*,#2282,.F.);
#2946=ORIENTED_EDGE('',*,*,#2295,.F.);
#2947=ORIENTED_EDGE('',*,*,#2306,.T.);
#2948=ORIENTED_EDGE('',*,*,#2296,.T.);
#2949=ORIENTED_EDGE('',*,*,#2292,.F.);
#2950=ORIENTED_EDGE('',*,*,#2307,.F.);
#2951=ORIENTED_EDGE('',*,*,#2308,.T.);
#2952=ORIENTED_EDGE('',*,*,#2307,.T.);
#2953=ORIENTED_EDGE('',*,*,#2291,.F.);
#2954=ORIENTED_EDGE('',*,*,#2309,.F.);
#2955=ORIENTED_EDGE('',*,*,#2310,.T.);
#2956=ORIENTED_EDGE('',*,*,#2309,.T.);
#2957=ORIENTED_EDGE('',*,*,#2290,.F.);
#2958=ORIENTED_EDGE('',*,*,#2311,.F.);
#2959=ORIENTED_EDGE('',*,*,#2312,.T.);
#2960=ORIENTED_EDGE('',*,*,#2311,.T.);
#2961=ORIENTED_EDGE('',*,*,#2289,.F.);
#2962=ORIENTED_EDGE('',*,*,#2313,.F.);
#2963=ORIENTED_EDGE('',*,*,#2276,.T.);
#2964=ORIENTED_EDGE('',*,*,#2314,.T.);
#2965=ORIENTED_EDGE('',*,*,#2313,.T.);
#2966=ORIENTED_EDGE('',*,*,#2288,.F.);
#2967=ORIENTED_EDGE('',*,*,#2315,.F.);
#2968=ORIENTED_EDGE('',*,*,#2316,.T.);
#2969=ORIENTED_EDGE('',*,*,#2315,.T.);
#2970=ORIENTED_EDGE('',*,*,#2287,.F.);
#2971=ORIENTED_EDGE('',*,*,#2317,.F.);
#2972=ORIENTED_EDGE('',*,*,#2271,.T.);
#2973=ORIENTED_EDGE('',*,*,#2274,.T.);
#2974=ORIENTED_EDGE('',*,*,#2318,.T.);
#2975=ORIENTED_EDGE('',*,*,#2317,.T.);
#2976=ORIENTED_EDGE('',*,*,#2286,.F.);
#2977=ORIENTED_EDGE('',*,*,#2299,.F.);
#2978=ORIENTED_EDGE('',*,*,#2280,.T.);
#2979=ORIENTED_EDGE('',*,*,#2297,.F.);
#2980=ORIENTED_EDGE('',*,*,#2306,.F.);
#2981=ORIENTED_EDGE('',*,*,#2308,.F.);
#2982=ORIENTED_EDGE('',*,*,#2310,.F.);
#2983=ORIENTED_EDGE('',*,*,#2312,.F.);
#2984=ORIENTED_EDGE('',*,*,#2314,.F.);
#2985=ORIENTED_EDGE('',*,*,#2316,.F.);
#2986=ORIENTED_EDGE('',*,*,#2318,.F.);
#2987=ORIENTED_EDGE('',*,*,#2298,.F.);
#2988=ORIENTED_EDGE('',*,*,#2301,.F.);
#2989=ORIENTED_EDGE('',*,*,#2303,.F.);
#2990=ORIENTED_EDGE('',*,*,#2305,.F.);
#2991=ORIENTED_EDGE('',*,*,#2294,.F.);
#2992=ORIENTED_EDGE('',*,*,#2319,.F.);
#2993=ORIENTED_EDGE('',*,*,#2320,.T.);
#2994=ORIENTED_EDGE('',*,*,#2321,.F.);
#2995=ORIENTED_EDGE('',*,*,#2322,.F.);
#2996=ORIENTED_EDGE('',*,*,#2323,.F.);
#2997=ORIENTED_EDGE('',*,*,#2324,.F.);
#2998=ORIENTED_EDGE('',*,*,#2320,.F.);
#2999=ORIENTED_EDGE('',*,*,#2325,.F.);
#3000=ORIENTED_EDGE('',*,*,#2326,.T.);
#3001=ORIENTED_EDGE('',*,*,#2327,.F.);
#3002=ORIENTED_EDGE('',*,*,#2328,.F.);
#3003=ORIENTED_EDGE('',*,*,#2329,.F.);
#3004=ORIENTED_EDGE('',*,*,#2330,.F.);
#3005=ORIENTED_EDGE('',*,*,#2326,.F.);
#3006=ORIENTED_EDGE('',*,*,#2322,.T.);
#3007=ORIENTED_EDGE('',*,*,#2319,.T.);
#3008=ORIENTED_EDGE('',*,*,#2324,.T.);
#3009=ORIENTED_EDGE('',*,*,#2331,.F.);
#3010=ORIENTED_EDGE('',*,*,#2332,.F.);
#3011=ORIENTED_EDGE('',*,*,#2333,.T.);
#3012=ORIENTED_EDGE('',*,*,#2334,.T.);
#3013=ORIENTED_EDGE('',*,*,#2335,.F.);
#3014=ORIENTED_EDGE('',*,*,#2328,.T.);
#3015=ORIENTED_EDGE('',*,*,#2325,.T.);
#3016=ORIENTED_EDGE('',*,*,#2330,.T.);
#3017=ORIENTED_EDGE('',*,*,#2336,.F.);
#3018=ORIENTED_EDGE('',*,*,#2337,.F.);
#3019=ORIENTED_EDGE('',*,*,#2338,.T.);
#3020=ORIENTED_EDGE('',*,*,#2339,.T.);
#3021=ORIENTED_EDGE('',*,*,#2340,.F.);
#3022=ORIENTED_EDGE('',*,*,#2341,.F.);
#3023=ORIENTED_EDGE('',*,*,#2342,.T.);
#3024=ORIENTED_EDGE('',*,*,#2321,.T.);
#3025=ORIENTED_EDGE('',*,*,#2342,.F.);
#3026=ORIENTED_EDGE('',*,*,#2343,.F.);
#3027=ORIENTED_EDGE('',*,*,#2344,.T.);
#3028=ORIENTED_EDGE('',*,*,#2327,.T.);
#3029=ORIENTED_EDGE('',*,*,#2344,.F.);
#3030=ORIENTED_EDGE('',*,*,#2345,.F.);
#3031=ORIENTED_EDGE('',*,*,#2346,.F.);
#3032=ORIENTED_EDGE('',*,*,#2347,.F.);
#3033=ORIENTED_EDGE('',*,*,#2348,.F.);
#3034=ORIENTED_EDGE('',*,*,#2347,.T.);
#3035=ORIENTED_EDGE('',*,*,#2349,.T.);
#3036=ORIENTED_EDGE('',*,*,#2337,.T.);
#3037=ORIENTED_EDGE('',*,*,#2350,.F.);
#3038=ORIENTED_EDGE('',*,*,#2334,.F.);
#3039=ORIENTED_EDGE('',*,*,#2351,.T.);
#3040=ORIENTED_EDGE('',*,*,#2346,.T.);
#3041=ORIENTED_EDGE('',*,*,#2352,.F.);
#3042=ORIENTED_EDGE('',*,*,#2338,.F.);
#3043=ORIENTED_EDGE('',*,*,#2349,.F.);
#3044=ORIENTED_EDGE('',*,*,#2343,.T.);
#3045=ORIENTED_EDGE('',*,*,#2345,.T.);
#3046=ORIENTED_EDGE('',*,*,#2353,.T.);
#3047=ORIENTED_EDGE('',*,*,#2332,.T.);
#3048=ORIENTED_EDGE('',*,*,#2354,.F.);
#3049=ORIENTED_EDGE('',*,*,#2339,.F.);
#3050=ORIENTED_EDGE('',*,*,#2352,.T.);
#3051=ORIENTED_EDGE('',*,*,#2323,.T.);
#3052=ORIENTED_EDGE('',*,*,#2335,.T.);
#3053=ORIENTED_EDGE('',*,*,#2350,.T.);
#3054=ORIENTED_EDGE('',*,*,#2336,.T.);
#3055=ORIENTED_EDGE('',*,*,#2329,.T.);
#3056=ORIENTED_EDGE('',*,*,#2340,.T.);
#3057=ORIENTED_EDGE('',*,*,#2354,.T.);
#3058=ORIENTED_EDGE('',*,*,#2331,.T.);
#3059=ORIENTED_EDGE('',*,*,#2348,.T.);
#3060=ORIENTED_EDGE('',*,*,#2351,.F.);
#3061=ORIENTED_EDGE('',*,*,#2333,.F.);
#3062=ORIENTED_EDGE('',*,*,#2353,.F.);
#3063=ORIENTED_EDGE('',*,*,#2341,.T.);
#3064=ORIENTED_EDGE('',*,*,#2355,.F.);
#3065=ORIENTED_EDGE('',*,*,#2356,.T.);
#3066=ORIENTED_EDGE('',*,*,#2357,.T.);
#3067=ORIENTED_EDGE('',*,*,#2356,.F.);
#3068=ORIENTED_EDGE('',*,*,#2357,.F.);
#3069=ORIENTED_EDGE('',*,*,#2358,.F.);
#3070=ORIENTED_EDGE('',*,*,#2359,.F.);
#3071=ORIENTED_EDGE('',*,*,#2360,.T.);
#3072=ORIENTED_EDGE('',*,*,#2358,.T.);
#3073=ORIENTED_EDGE('',*,*,#2360,.F.);
#3074=ORIENTED_EDGE('',*,*,#2361,.F.);
#3075=ORIENTED_EDGE('',*,*,#2362,.T.);
#3076=ORIENTED_EDGE('',*,*,#2363,.T.);
#3077=ORIENTED_EDGE('',*,*,#2362,.F.);
#3078=ORIENTED_EDGE('',*,*,#2361,.T.);
#3079=ORIENTED_EDGE('',*,*,#2359,.T.);
#3080=ORIENTED_EDGE('',*,*,#2363,.F.);
#3081=ORIENTED_EDGE('',*,*,#2355,.T.);
#3082=ORIENTED_EDGE('',*,*,#2364,.F.);
#3083=ORIENTED_EDGE('',*,*,#2365,.T.);
#3084=ORIENTED_EDGE('',*,*,#2366,.F.);
#3085=ORIENTED_EDGE('',*,*,#2365,.F.);
#3086=ORIENTED_EDGE('',*,*,#2367,.F.);
#3087=ORIENTED_EDGE('',*,*,#2368,.T.);
#3088=ORIENTED_EDGE('',*,*,#2369,.F.);
#3089=ORIENTED_EDGE('',*,*,#2368,.F.);
#3090=ORIENTED_EDGE('',*,*,#2370,.F.);
#3091=ORIENTED_EDGE('',*,*,#2371,.T.);
#3092=ORIENTED_EDGE('',*,*,#2372,.F.);
#3093=ORIENTED_EDGE('',*,*,#2371,.F.);
#3094=ORIENTED_EDGE('',*,*,#2373,.F.);
#3095=ORIENTED_EDGE('',*,*,#2374,.T.);
#3096=ORIENTED_EDGE('',*,*,#2375,.F.);
#3097=ORIENTED_EDGE('',*,*,#2374,.F.);
#3098=ORIENTED_EDGE('',*,*,#2376,.F.);
#3099=ORIENTED_EDGE('',*,*,#2377,.F.);
#3100=ORIENTED_EDGE('',*,*,#2373,.T.);
#3101=ORIENTED_EDGE('',*,*,#2370,.T.);
#3102=ORIENTED_EDGE('',*,*,#2367,.T.);
#3103=ORIENTED_EDGE('',*,*,#2364,.T.);
#3104=ORIENTED_EDGE('',*,*,#2378,.F.);
#3105=ORIENTED_EDGE('',*,*,#2379,.T.);
#3106=ORIENTED_EDGE('',*,*,#2376,.T.);
#3107=ORIENTED_EDGE('',*,*,#2379,.F.);
#3108=ORIENTED_EDGE('',*,*,#2380,.F.);
#3109=ORIENTED_EDGE('',*,*,#2381,.T.);
#3110=ORIENTED_EDGE('',*,*,#2382,.T.);
#3111=ORIENTED_EDGE('',*,*,#2381,.F.);
#3112=ORIENTED_EDGE('',*,*,#2377,.T.);
#3113=ORIENTED_EDGE('',*,*,#2383,.T.);
#3114=ORIENTED_EDGE('',*,*,#2384,.T.);
#3115=ORIENTED_EDGE('',*,*,#2383,.F.);
#3116=ORIENTED_EDGE('',*,*,#2378,.T.);
#3117=ORIENTED_EDGE('',*,*,#2380,.T.);
#3118=ORIENTED_EDGE('',*,*,#2375,.T.);
#3119=ORIENTED_EDGE('',*,*,#2372,.T.);
#3120=ORIENTED_EDGE('',*,*,#2369,.T.);
#3121=ORIENTED_EDGE('',*,*,#2366,.T.);
#3122=ORIENTED_EDGE('',*,*,#2384,.F.);
#3123=ORIENTED_EDGE('',*,*,#2382,.F.);
#3124=ORIENTED_EDGE('',*,*,#2385,.F.);
#3125=ORIENTED_EDGE('',*,*,#2386,.T.);
#3126=ORIENTED_EDGE('',*,*,#2387,.F.);
#3127=ORIENTED_EDGE('',*,*,#2386,.F.);
#3128=ORIENTED_EDGE('',*,*,#2385,.T.);
#3129=ORIENTED_EDGE('',*,*,#2388,.F.);
#3130=ORIENTED_EDGE('',*,*,#2388,.T.);
#3131=ORIENTED_EDGE('',*,*,#2389,.T.);
#3132=ORIENTED_EDGE('',*,*,#2390,.T.);
#3133=ORIENTED_EDGE('',*,*,#2389,.F.);
#3134=ORIENTED_EDGE('',*,*,#2391,.F.);
#3135=ORIENTED_EDGE('',*,*,#2392,.T.);
#3136=ORIENTED_EDGE('',*,*,#2393,.T.);
#3137=ORIENTED_EDGE('',*,*,#2392,.F.);
#3138=ORIENTED_EDGE('',*,*,#2391,.T.);
#3139=ORIENTED_EDGE('',*,*,#2387,.T.);
#3140=ORIENTED_EDGE('',*,*,#2393,.F.);
#3141=ORIENTED_EDGE('',*,*,#2390,.F.);
#3142=ORIENTED_EDGE('',*,*,#2394,.F.);
#3143=ORIENTED_EDGE('',*,*,#2395,.T.);
#3144=ORIENTED_EDGE('',*,*,#2396,.F.);
#3145=ORIENTED_EDGE('',*,*,#2395,.F.);
#3146=ORIENTED_EDGE('',*,*,#2397,.F.);
#3147=ORIENTED_EDGE('',*,*,#2398,.T.);
#3148=ORIENTED_EDGE('',*,*,#2399,.F.);
#3149=ORIENTED_EDGE('',*,*,#2398,.F.);
#3150=ORIENTED_EDGE('',*,*,#2400,.F.);
#3151=ORIENTED_EDGE('',*,*,#2401,.T.);
#3152=ORIENTED_EDGE('',*,*,#2402,.F.);
#3153=ORIENTED_EDGE('',*,*,#2401,.F.);
#3154=ORIENTED_EDGE('',*,*,#2403,.F.);
#3155=ORIENTED_EDGE('',*,*,#2404,.T.);
#3156=ORIENTED_EDGE('',*,*,#2405,.F.);
#3157=ORIENTED_EDGE('',*,*,#2404,.F.);
#3158=ORIENTED_EDGE('',*,*,#2406,.T.);
#3159=ORIENTED_EDGE('',*,*,#2407,.F.);
#3160=ORIENTED_EDGE('',*,*,#2405,.T.);
#3161=ORIENTED_EDGE('',*,*,#2402,.T.);
#3162=ORIENTED_EDGE('',*,*,#2399,.T.);
#3163=ORIENTED_EDGE('',*,*,#2396,.T.);
#3164=ORIENTED_EDGE('',*,*,#2406,.F.);
#3165=ORIENTED_EDGE('',*,*,#2408,.T.);
#3166=ORIENTED_EDGE('',*,*,#2409,.T.);
#3167=ORIENTED_EDGE('',*,*,#2408,.F.);
#3168=ORIENTED_EDGE('',*,*,#2410,.F.);
#3169=ORIENTED_EDGE('',*,*,#2411,.T.);
#3170=ORIENTED_EDGE('',*,*,#2412,.T.);
#3171=ORIENTED_EDGE('',*,*,#2411,.F.);
#3172=ORIENTED_EDGE('',*,*,#2413,.F.);
#3173=ORIENTED_EDGE('',*,*,#2414,.T.);
#3174=ORIENTED_EDGE('',*,*,#2407,.T.);
#3175=ORIENTED_EDGE('',*,*,#2414,.F.);
#3176=ORIENTED_EDGE('',*,*,#2413,.T.);
#3177=ORIENTED_EDGE('',*,*,#2410,.T.);
#3178=ORIENTED_EDGE('',*,*,#2409,.F.);
#3179=ORIENTED_EDGE('',*,*,#2412,.F.);
#3180=ORIENTED_EDGE('',*,*,#2403,.T.);
#3181=ORIENTED_EDGE('',*,*,#2400,.T.);
#3182=ORIENTED_EDGE('',*,*,#2397,.T.);
#3183=ORIENTED_EDGE('',*,*,#2394,.T.);
#3184=ORIENTED_EDGE('',*,*,#2415,.F.);
#3185=ORIENTED_EDGE('',*,*,#2416,.T.);
#3186=ORIENTED_EDGE('',*,*,#2417,.T.);
#3187=ORIENTED_EDGE('',*,*,#2416,.F.);
#3188=ORIENTED_EDGE('',*,*,#2418,.F.);
#3189=ORIENTED_EDGE('',*,*,#2419,.T.);
#3190=ORIENTED_EDGE('',*,*,#2420,.T.);
#3191=ORIENTED_EDGE('',*,*,#2419,.F.);
#3192=ORIENTED_EDGE('',*,*,#2418,.T.);
#3193=ORIENTED_EDGE('',*,*,#2415,.T.);
#3194=ORIENTED_EDGE('',*,*,#2420,.F.);
#3195=ORIENTED_EDGE('',*,*,#2417,.F.);
#3196=ORIENTED_EDGE('',*,*,#2421,.T.);
#3197=ORIENTED_EDGE('',*,*,#2422,.T.);
#3198=ORIENTED_EDGE('',*,*,#2423,.T.);
#3199=ORIENTED_EDGE('',*,*,#2424,.F.);
#3200=ORIENTED_EDGE('',*,*,#2425,.T.);
#3201=ORIENTED_EDGE('',*,*,#2426,.T.);
#3202=ORIENTED_EDGE('',*,*,#2427,.T.);
#3203=ORIENTED_EDGE('',*,*,#2422,.F.);
#3204=ORIENTED_EDGE('',*,*,#2428,.T.);
#3205=ORIENTED_EDGE('',*,*,#2429,.T.);
#3206=ORIENTED_EDGE('',*,*,#2430,.T.);
#3207=ORIENTED_EDGE('',*,*,#2426,.F.);
#3208=ORIENTED_EDGE('',*,*,#2431,.T.);
#3209=ORIENTED_EDGE('',*,*,#2432,.T.);
#3210=ORIENTED_EDGE('',*,*,#2433,.T.);
#3211=ORIENTED_EDGE('',*,*,#2429,.F.);
#3212=ORIENTED_EDGE('',*,*,#2434,.T.);
#3213=ORIENTED_EDGE('',*,*,#2435,.T.);
#3214=ORIENTED_EDGE('',*,*,#2436,.T.);
#3215=ORIENTED_EDGE('',*,*,#2432,.F.);
#3216=ORIENTED_EDGE('',*,*,#2437,.T.);
#3217=ORIENTED_EDGE('',*,*,#2424,.T.);
#3218=ORIENTED_EDGE('',*,*,#2438,.T.);
#3219=ORIENTED_EDGE('',*,*,#2435,.F.);
#3220=ORIENTED_EDGE('',*,*,#2437,.F.);
#3221=ORIENTED_EDGE('',*,*,#2434,.F.);
#3222=ORIENTED_EDGE('',*,*,#2431,.F.);
#3223=ORIENTED_EDGE('',*,*,#2428,.F.);
#3224=ORIENTED_EDGE('',*,*,#2425,.F.);
#3225=ORIENTED_EDGE('',*,*,#2421,.F.);
#3226=ORIENTED_EDGE('',*,*,#2438,.F.);
#3227=ORIENTED_EDGE('',*,*,#2423,.F.);
#3228=ORIENTED_EDGE('',*,*,#2427,.F.);
#3229=ORIENTED_EDGE('',*,*,#2430,.F.);
#3230=ORIENTED_EDGE('',*,*,#2433,.F.);
#3231=ORIENTED_EDGE('',*,*,#2436,.F.);
#3232=ORIENTED_EDGE('',*,*,#2439,.F.);
#3233=ORIENTED_EDGE('',*,*,#2440,.F.);
#3234=ORIENTED_EDGE('',*,*,#2441,.F.);
#3235=ORIENTED_EDGE('',*,*,#2442,.T.);
#3236=ORIENTED_EDGE('',*,*,#2440,.T.);
#3237=ORIENTED_EDGE('',*,*,#2442,.F.);
#3238=ORIENTED_EDGE('',*,*,#2443,.F.);
#3239=ORIENTED_EDGE('',*,*,#2444,.T.);
#3240=ORIENTED_EDGE('',*,*,#2441,.T.);
#3241=ORIENTED_EDGE('',*,*,#2444,.F.);
#3242=ORIENTED_EDGE('',*,*,#2445,.F.);
#3243=ORIENTED_EDGE('',*,*,#2446,.T.);
#3244=ORIENTED_EDGE('',*,*,#2443,.T.);
#3245=ORIENTED_EDGE('',*,*,#2446,.F.);
#3246=ORIENTED_EDGE('',*,*,#2445,.T.);
#3247=ORIENTED_EDGE('',*,*,#2447,.F.);
#3248=ORIENTED_EDGE('',*,*,#2448,.F.);
#3249=ORIENTED_EDGE('',*,*,#2449,.T.);
#3250=ORIENTED_EDGE('',*,*,#2447,.T.);
#3251=ORIENTED_EDGE('',*,*,#2449,.F.);
#3252=ORIENTED_EDGE('',*,*,#2439,.T.);
#3253=ORIENTED_EDGE('',*,*,#2450,.T.);
#3254=ORIENTED_EDGE('',*,*,#2448,.T.);
#3255=ORIENTED_EDGE('',*,*,#2450,.F.);
#3256=ORIENTED_EDGE('',*,*,#2451,.F.);
#3257=ORIENTED_EDGE('',*,*,#2452,.F.);
#3258=ORIENTED_EDGE('',*,*,#2453,.T.);
#3259=ORIENTED_EDGE('',*,*,#2451,.T.);
#3260=ORIENTED_EDGE('',*,*,#2453,.F.);
#3261=ORIENTED_EDGE('',*,*,#2454,.F.);
#3262=ORIENTED_EDGE('',*,*,#2455,.T.);
#3263=ORIENTED_EDGE('',*,*,#2452,.T.);
#3264=ORIENTED_EDGE('',*,*,#2455,.F.);
#3265=ORIENTED_EDGE('',*,*,#2456,.F.);
#3266=ORIENTED_EDGE('',*,*,#2457,.T.);
#3267=ORIENTED_EDGE('',*,*,#2454,.T.);
#3268=ORIENTED_EDGE('',*,*,#2457,.F.);
#3269=ORIENTED_EDGE('',*,*,#2456,.T.);
#3270=ORIENTED_EDGE('',*,*,#2458,.F.);
#3271=ORIENTED_EDGE('',*,*,#2459,.F.);
#3272=ORIENTED_EDGE('',*,*,#2460,.T.);
#3273=ORIENTED_EDGE('',*,*,#2458,.T.);
#3274=ORIENTED_EDGE('',*,*,#2460,.F.);
#3275=ORIENTED_EDGE('',*,*,#2461,.F.);
#3276=ORIENTED_EDGE('',*,*,#2462,.T.);
#3277=ORIENTED_EDGE('',*,*,#2459,.T.);
#3278=ORIENTED_EDGE('',*,*,#2462,.F.);
#3279=ORIENTED_EDGE('',*,*,#2463,.F.);
#3280=ORIENTED_EDGE('',*,*,#2464,.T.);
#3281=ORIENTED_EDGE('',*,*,#2461,.T.);
#3282=ORIENTED_EDGE('',*,*,#2464,.F.);
#3283=ORIENTED_EDGE('',*,*,#2463,.T.);
#3284=ORIENTED_EDGE('',*,*,#2465,.T.);
#3285=ORIENTED_EDGE('',*,*,#2466,.T.);
#3286=ORIENTED_EDGE('',*,*,#2467,.T.);
#3287=ORIENTED_EDGE('',*,*,#2468,.F.);
#3288=ORIENTED_EDGE('',*,*,#2469,.T.);
#3289=ORIENTED_EDGE('',*,*,#2470,.T.);
#3290=ORIENTED_EDGE('',*,*,#2471,.T.);
#3291=ORIENTED_EDGE('',*,*,#2466,.F.);
#3292=ORIENTED_EDGE('',*,*,#2472,.T.);
#3293=ORIENTED_EDGE('',*,*,#2473,.T.);
#3294=ORIENTED_EDGE('',*,*,#2474,.T.);
#3295=ORIENTED_EDGE('',*,*,#2470,.F.);
#3296=ORIENTED_EDGE('',*,*,#2475,.T.);
#3297=ORIENTED_EDGE('',*,*,#2476,.T.);
#3298=ORIENTED_EDGE('',*,*,#2477,.T.);
#3299=ORIENTED_EDGE('',*,*,#2473,.F.);
#3300=ORIENTED_EDGE('',*,*,#2478,.T.);
#3301=ORIENTED_EDGE('',*,*,#2479,.T.);
#3302=ORIENTED_EDGE('',*,*,#2480,.T.);
#3303=ORIENTED_EDGE('',*,*,#2476,.F.);
#3304=ORIENTED_EDGE('',*,*,#2481,.T.);
#3305=ORIENTED_EDGE('',*,*,#2468,.T.);
#3306=ORIENTED_EDGE('',*,*,#2482,.T.);
#3307=ORIENTED_EDGE('',*,*,#2479,.F.);
#3308=ORIENTED_EDGE('',*,*,#2481,.F.);
#3309=ORIENTED_EDGE('',*,*,#2478,.F.);
#3310=ORIENTED_EDGE('',*,*,#2475,.F.);
#3311=ORIENTED_EDGE('',*,*,#2472,.F.);
#3312=ORIENTED_EDGE('',*,*,#2469,.F.);
#3313=ORIENTED_EDGE('',*,*,#2465,.F.);
#3314=ORIENTED_EDGE('',*,*,#2482,.F.);
#3315=ORIENTED_EDGE('',*,*,#2467,.F.);
#3316=ORIENTED_EDGE('',*,*,#2471,.F.);
#3317=ORIENTED_EDGE('',*,*,#2474,.F.);
#3318=ORIENTED_EDGE('',*,*,#2477,.F.);
#3319=ORIENTED_EDGE('',*,*,#2480,.F.);
#3320=ORIENTED_EDGE('',*,*,#2483,.F.);
#3321=ORIENTED_EDGE('',*,*,#2484,.F.);
#3322=ORIENTED_EDGE('',*,*,#2485,.T.);
#3323=ORIENTED_EDGE('',*,*,#2486,.F.);
#3324=ORIENTED_EDGE('',*,*,#2485,.F.);
#3325=ORIENTED_EDGE('',*,*,#2487,.F.);
#3326=ORIENTED_EDGE('',*,*,#2488,.T.);
#3327=ORIENTED_EDGE('',*,*,#2488,.F.);
#3328=ORIENTED_EDGE('',*,*,#2487,.T.);
#3329=ORIENTED_EDGE('',*,*,#2484,.T.);
#3330=ORIENTED_EDGE('',*,*,#2489,.T.);
#3331=ORIENTED_EDGE('',*,*,#2490,.T.);
#3332=ORIENTED_EDGE('',*,*,#2483,.T.);
#3333=ORIENTED_EDGE('',*,*,#2490,.F.);
#3334=ORIENTED_EDGE('',*,*,#2491,.T.);
#3335=ORIENTED_EDGE('',*,*,#2492,.F.);
#3336=ORIENTED_EDGE('',*,*,#2491,.F.);
#3337=ORIENTED_EDGE('',*,*,#2489,.F.);
#3338=ORIENTED_EDGE('',*,*,#2493,.F.);
#3339=ORIENTED_EDGE('',*,*,#2486,.T.);
#3340=ORIENTED_EDGE('',*,*,#2494,.F.);
#3341=ORIENTED_EDGE('',*,*,#2495,.T.);
#3342=ORIENTED_EDGE('',*,*,#2493,.T.);
#3343=ORIENTED_EDGE('',*,*,#2495,.F.);
#3344=ORIENTED_EDGE('',*,*,#2496,.F.);
#3345=ORIENTED_EDGE('',*,*,#2497,.T.);
#3346=ORIENTED_EDGE('',*,*,#2498,.F.);
#3347=ORIENTED_EDGE('',*,*,#2497,.F.);
#3348=ORIENTED_EDGE('',*,*,#2496,.T.);
#3349=ORIENTED_EDGE('',*,*,#2492,.T.);
#3350=ORIENTED_EDGE('',*,*,#2499,.T.);
#3351=ORIENTED_EDGE('',*,*,#2500,.T.);
#3352=ORIENTED_EDGE('',*,*,#2501,.F.);
#3353=ORIENTED_EDGE('',*,*,#2502,.F.);
#3354=ORIENTED_EDGE('',*,*,#2503,.F.);
#3355=ORIENTED_EDGE('',*,*,#2500,.F.);
#3356=ORIENTED_EDGE('',*,*,#2504,.T.);
#3357=ORIENTED_EDGE('',*,*,#2505,.T.);
#3358=ORIENTED_EDGE('',*,*,#2504,.F.);
#3359=ORIENTED_EDGE('',*,*,#2499,.F.);
#3360=ORIENTED_EDGE('',*,*,#2506,.F.);
#3361=ORIENTED_EDGE('',*,*,#2494,.T.);
#3362=ORIENTED_EDGE('',*,*,#2507,.F.);
#3363=ORIENTED_EDGE('',*,*,#2508,.T.);
#3364=ORIENTED_EDGE('',*,*,#2506,.T.);
#3365=ORIENTED_EDGE('',*,*,#2508,.F.);
#3366=ORIENTED_EDGE('',*,*,#2507,.T.);
#3367=ORIENTED_EDGE('',*,*,#2505,.F.);
#3368=ORIENTED_EDGE('',*,*,#2509,.F.);
#3369=ORIENTED_EDGE('',*,*,#2510,.T.);
#3370=ORIENTED_EDGE('',*,*,#2511,.F.);
#3371=ORIENTED_EDGE('',*,*,#2512,.T.);
#3372=ORIENTED_EDGE('',*,*,#2509,.T.);
#3373=ORIENTED_EDGE('',*,*,#2512,.F.);
#3374=ORIENTED_EDGE('',*,*,#2511,.T.);
#3375=ORIENTED_EDGE('',*,*,#2498,.T.);
#3376=ORIENTED_EDGE('',*,*,#2510,.F.);
#3377=ORIENTED_EDGE('',*,*,#2513,.T.);
#3378=ORIENTED_EDGE('',*,*,#2501,.T.);
#3379=ORIENTED_EDGE('',*,*,#2503,.T.);
#3380=ORIENTED_EDGE('',*,*,#2502,.T.);
#3381=ORIENTED_EDGE('',*,*,#2513,.F.);
#3382=ORIENTED_EDGE('',*,*,#2514,.T.);
#3383=ORIENTED_EDGE('',*,*,#2515,.T.);
#3384=ORIENTED_EDGE('',*,*,#2516,.T.);
#3385=ORIENTED_EDGE('',*,*,#2517,.T.);
#3386=ORIENTED_EDGE('',*,*,#2518,.T.);
#3387=ORIENTED_EDGE('',*,*,#2519,.T.);
#3388=ORIENTED_EDGE('',*,*,#2520,.F.);
#3389=ORIENTED_EDGE('',*,*,#2521,.T.);
#3390=ORIENTED_EDGE('',*,*,#2522,.T.);
#3391=ORIENTED_EDGE('',*,*,#2523,.T.);
#3392=ORIENTED_EDGE('',*,*,#2524,.T.);
#3393=ORIENTED_EDGE('',*,*,#2525,.T.);
#3394=ORIENTED_EDGE('',*,*,#2526,.T.);
#3395=ORIENTED_EDGE('',*,*,#2527,.F.);
#3396=ORIENTED_EDGE('',*,*,#2528,.F.);
#3397=ORIENTED_EDGE('',*,*,#2526,.F.);
#3398=ORIENTED_EDGE('',*,*,#2529,.F.);
#3399=ORIENTED_EDGE('',*,*,#2515,.F.);
#3400=ORIENTED_EDGE('',*,*,#2529,.T.);
#3401=ORIENTED_EDGE('',*,*,#2525,.F.);
#3402=ORIENTED_EDGE('',*,*,#2530,.F.);
#3403=ORIENTED_EDGE('',*,*,#2516,.F.);
#3404=ORIENTED_EDGE('',*,*,#2530,.T.);
#3405=ORIENTED_EDGE('',*,*,#2524,.F.);
#3406=ORIENTED_EDGE('',*,*,#2531,.F.);
#3407=ORIENTED_EDGE('',*,*,#2517,.F.);
#3408=ORIENTED_EDGE('',*,*,#2531,.T.);
#3409=ORIENTED_EDGE('',*,*,#2523,.F.);
#3410=ORIENTED_EDGE('',*,*,#2532,.F.);
#3411=ORIENTED_EDGE('',*,*,#2518,.F.);
#3412=ORIENTED_EDGE('',*,*,#2532,.T.);
#3413=ORIENTED_EDGE('',*,*,#2522,.F.);
#3414=ORIENTED_EDGE('',*,*,#2533,.F.);
#3415=ORIENTED_EDGE('',*,*,#2519,.F.);
#3416=ORIENTED_EDGE('',*,*,#2533,.T.);
#3417=ORIENTED_EDGE('',*,*,#2521,.F.);
#3418=ORIENTED_EDGE('',*,*,#2528,.T.);
#3419=ORIENTED_EDGE('',*,*,#2514,.F.);
#3420=ORIENTED_EDGE('',*,*,#2527,.T.);
#3421=ORIENTED_EDGE('',*,*,#2534,.T.);
#3422=ORIENTED_EDGE('',*,*,#2535,.T.);
#3423=ORIENTED_EDGE('',*,*,#2534,.F.);
#3424=ORIENTED_EDGE('',*,*,#2536,.F.);
#3425=ORIENTED_EDGE('',*,*,#2537,.T.);
#3426=ORIENTED_EDGE('',*,*,#2535,.F.);
#3427=ORIENTED_EDGE('',*,*,#2538,.T.);
#3428=ORIENTED_EDGE('',*,*,#2536,.T.);
#3429=ORIENTED_EDGE('',*,*,#2538,.F.);
#3430=ORIENTED_EDGE('',*,*,#2539,.F.);
#3431=ORIENTED_EDGE('',*,*,#2540,.T.);
#3432=ORIENTED_EDGE('',*,*,#2520,.T.);
#3433=ORIENTED_EDGE('',*,*,#2540,.F.);
#3434=ORIENTED_EDGE('',*,*,#2541,.F.);
#3435=ORIENTED_EDGE('',*,*,#2542,.T.);
#3436=ORIENTED_EDGE('',*,*,#2539,.T.);
#3437=ORIENTED_EDGE('',*,*,#2542,.F.);
#3438=ORIENTED_EDGE('',*,*,#2541,.T.);
#3439=ORIENTED_EDGE('',*,*,#2543,.F.);
#3440=ORIENTED_EDGE('',*,*,#2543,.T.);
#3441=ORIENTED_EDGE('',*,*,#2544,.T.);
#3442=ORIENTED_EDGE('',*,*,#2537,.F.);
#3443=ORIENTED_EDGE('',*,*,#2544,.F.);
#3444=ORIENTED_EDGE('',*,*,#2545,.F.);
#3445=ORIENTED_EDGE('',*,*,#2546,.F.);
#3446=ORIENTED_EDGE('',*,*,#2547,.T.);
#3447=ORIENTED_EDGE('',*,*,#2545,.T.);
#3448=ORIENTED_EDGE('',*,*,#2547,.F.);
#3449=ORIENTED_EDGE('',*,*,#2548,.F.);
#3450=ORIENTED_EDGE('',*,*,#2549,.T.);
#3451=ORIENTED_EDGE('',*,*,#2546,.T.);
#3452=ORIENTED_EDGE('',*,*,#2549,.F.);
#3453=ORIENTED_EDGE('',*,*,#2550,.F.);
#3454=ORIENTED_EDGE('',*,*,#2551,.T.);
#3455=ORIENTED_EDGE('',*,*,#2548,.T.);
#3456=ORIENTED_EDGE('',*,*,#2551,.F.);
#3457=ORIENTED_EDGE('',*,*,#2550,.T.);
#3458=ORIENTED_EDGE('',*,*,#2552,.F.);
#3459=ORIENTED_EDGE('',*,*,#2553,.F.);
#3460=ORIENTED_EDGE('',*,*,#2554,.T.);
#3461=ORIENTED_EDGE('',*,*,#2552,.T.);
#3462=ORIENTED_EDGE('',*,*,#2554,.F.);
#3463=ORIENTED_EDGE('',*,*,#2555,.F.);
#3464=ORIENTED_EDGE('',*,*,#2556,.T.);
#3465=ORIENTED_EDGE('',*,*,#2553,.T.);
#3466=ORIENTED_EDGE('',*,*,#2556,.F.);
#3467=ORIENTED_EDGE('',*,*,#2557,.F.);
#3468=ORIENTED_EDGE('',*,*,#2558,.T.);
#3469=ORIENTED_EDGE('',*,*,#2555,.T.);
#3470=ORIENTED_EDGE('',*,*,#2558,.F.);
#3471=ORIENTED_EDGE('',*,*,#2557,.T.);
#3472=ORIENTED_EDGE('',*,*,#2559,.T.);
#3473=ORIENTED_EDGE('',*,*,#2560,.T.);
#3474=ORIENTED_EDGE('',*,*,#2561,.T.);
#3475=ORIENTED_EDGE('',*,*,#2562,.F.);
#3476=ORIENTED_EDGE('',*,*,#2563,.T.);
#3477=ORIENTED_EDGE('',*,*,#2564,.T.);
#3478=ORIENTED_EDGE('',*,*,#2565,.T.);
#3479=ORIENTED_EDGE('',*,*,#2560,.F.);
#3480=ORIENTED_EDGE('',*,*,#2566,.T.);
#3481=ORIENTED_EDGE('',*,*,#2567,.T.);
#3482=ORIENTED_EDGE('',*,*,#2568,.T.);
#3483=ORIENTED_EDGE('',*,*,#2564,.F.);
#3484=ORIENTED_EDGE('',*,*,#2569,.T.);
#3485=ORIENTED_EDGE('',*,*,#2570,.T.);
#3486=ORIENTED_EDGE('',*,*,#2571,.T.);
#3487=ORIENTED_EDGE('',*,*,#2567,.F.);
#3488=ORIENTED_EDGE('',*,*,#2572,.T.);
#3489=ORIENTED_EDGE('',*,*,#2573,.T.);
#3490=ORIENTED_EDGE('',*,*,#2574,.T.);
#3491=ORIENTED_EDGE('',*,*,#2570,.F.);
#3492=ORIENTED_EDGE('',*,*,#2575,.T.);
#3493=ORIENTED_EDGE('',*,*,#2562,.T.);
#3494=ORIENTED_EDGE('',*,*,#2576,.T.);
#3495=ORIENTED_EDGE('',*,*,#2573,.F.);
#3496=ORIENTED_EDGE('',*,*,#2575,.F.);
#3497=ORIENTED_EDGE('',*,*,#2572,.F.);
#3498=ORIENTED_EDGE('',*,*,#2569,.F.);
#3499=ORIENTED_EDGE('',*,*,#2566,.F.);
#3500=ORIENTED_EDGE('',*,*,#2563,.F.);
#3501=ORIENTED_EDGE('',*,*,#2559,.F.);
#3502=ORIENTED_EDGE('',*,*,#2576,.F.);
#3503=ORIENTED_EDGE('',*,*,#2561,.F.);
#3504=ORIENTED_EDGE('',*,*,#2565,.F.);
#3505=ORIENTED_EDGE('',*,*,#2568,.F.);
#3506=ORIENTED_EDGE('',*,*,#2571,.F.);
#3507=ORIENTED_EDGE('',*,*,#2574,.F.);
#3508=ORIENTED_EDGE('',*,*,#2577,.F.);
#3509=ORIENTED_EDGE('',*,*,#2578,.T.);
#3510=ORIENTED_EDGE('',*,*,#2579,.T.);
#3511=ORIENTED_EDGE('',*,*,#2578,.F.);
#3512=ORIENTED_EDGE('',*,*,#2580,.F.);
#3513=ORIENTED_EDGE('',*,*,#2581,.T.);
#3514=ORIENTED_EDGE('',*,*,#2582,.T.);
#3515=ORIENTED_EDGE('',*,*,#2581,.F.);
#3516=ORIENTED_EDGE('',*,*,#2580,.T.);
#3517=ORIENTED_EDGE('',*,*,#2577,.T.);
#3518=ORIENTED_EDGE('',*,*,#2582,.F.);
#3519=ORIENTED_EDGE('',*,*,#2579,.F.);
#3520=ORIENTED_EDGE('',*,*,#2583,.F.);
#3521=ORIENTED_EDGE('',*,*,#2584,.F.);
#3522=ORIENTED_EDGE('',*,*,#2585,.T.);
#3523=ORIENTED_EDGE('',*,*,#2586,.F.);
#3524=ORIENTED_EDGE('',*,*,#2585,.F.);
#3525=ORIENTED_EDGE('',*,*,#2587,.F.);
#3526=ORIENTED_EDGE('',*,*,#2588,.F.);
#3527=ORIENTED_EDGE('',*,*,#2589,.F.);
#3528=ORIENTED_EDGE('',*,*,#2590,.F.);
#3529=ORIENTED_EDGE('',*,*,#2591,.F.);
#3530=ORIENTED_EDGE('',*,*,#2592,.T.);
#3531=ORIENTED_EDGE('',*,*,#2593,.F.);
#3532=ORIENTED_EDGE('',*,*,#2594,.F.);
#3533=ORIENTED_EDGE('',*,*,#2595,.F.);
#3534=ORIENTED_EDGE('',*,*,#2596,.F.);
#3535=ORIENTED_EDGE('',*,*,#2597,.F.);
#3536=ORIENTED_EDGE('',*,*,#2598,.F.);
#3537=ORIENTED_EDGE('',*,*,#2592,.F.);
#3538=ORIENTED_EDGE('',*,*,#2588,.T.);
#3539=ORIENTED_EDGE('',*,*,#2599,.T.);
#3540=ORIENTED_EDGE('',*,*,#2597,.T.);
#3541=ORIENTED_EDGE('',*,*,#2600,.F.);
#3542=ORIENTED_EDGE('',*,*,#2587,.T.);
#3543=ORIENTED_EDGE('',*,*,#2601,.T.);
#3544=ORIENTED_EDGE('',*,*,#2598,.T.);
#3545=ORIENTED_EDGE('',*,*,#2599,.F.);
#3546=ORIENTED_EDGE('',*,*,#2584,.T.);
#3547=ORIENTED_EDGE('',*,*,#2602,.T.);
#3548=ORIENTED_EDGE('',*,*,#2593,.T.);
#3549=ORIENTED_EDGE('',*,*,#2601,.F.);
#3550=ORIENTED_EDGE('',*,*,#2603,.F.);
#3551=ORIENTED_EDGE('',*,*,#2604,.T.);
#3552=ORIENTED_EDGE('',*,*,#2605,.T.);
#3553=ORIENTED_EDGE('',*,*,#2604,.F.);
#3554=ORIENTED_EDGE('',*,*,#2583,.T.);
#3555=ORIENTED_EDGE('',*,*,#2606,.T.);
#3556=ORIENTED_EDGE('',*,*,#2594,.T.);
#3557=ORIENTED_EDGE('',*,*,#2602,.F.);
#3558=ORIENTED_EDGE('',*,*,#2589,.T.);
#3559=ORIENTED_EDGE('',*,*,#2600,.T.);
#3560=ORIENTED_EDGE('',*,*,#2596,.T.);
#3561=ORIENTED_EDGE('',*,*,#2607,.F.);
#3562=ORIENTED_EDGE('',*,*,#2590,.T.);
#3563=ORIENTED_EDGE('',*,*,#2607,.T.);
#3564=ORIENTED_EDGE('',*,*,#2595,.T.);
#3565=ORIENTED_EDGE('',*,*,#2606,.F.);
#3566=ORIENTED_EDGE('',*,*,#2591,.T.);
#3567=ORIENTED_EDGE('',*,*,#2603,.T.);
#3568=ORIENTED_EDGE('',*,*,#2586,.T.);
#3569=ORIENTED_EDGE('',*,*,#2605,.F.);
#3570=CYLINDRICAL_SURFACE('',#4096,0.21);
#3571=CYLINDRICAL_SURFACE('',#4099,0.21);
#3572=CYLINDRICAL_SURFACE('',#4102,0.21);
#3573=CYLINDRICAL_SURFACE('',#4105,0.21);
#3574=CYLINDRICAL_SURFACE('',#4129,0.21);
#3575=CYLINDRICAL_SURFACE('',#4133,0.21);
#3576=CYLINDRICAL_SURFACE('',#4137,0.275);
#3577=CYLINDRICAL_SURFACE('',#4140,0.275);
#3578=CYLINDRICAL_SURFACE('',#4143,1.31);
#3579=CYLINDRICAL_SURFACE('',#4165,0.475);
#3580=CYLINDRICAL_SURFACE('',#4170,0.475);
#3581=CYLINDRICAL_SURFACE('',#4174,0.275);
#3582=CYLINDRICAL_SURFACE('',#4176,0.275);
#3583=CYLINDRICAL_SURFACE('',#4178,1.31);
#3584=CYLINDRICAL_SURFACE('',#4187,0.21);
#3585=CYLINDRICAL_SURFACE('',#4191,0.21);
#3586=CYLINDRICAL_SURFACE('',#4195,0.275);
#3587=CYLINDRICAL_SURFACE('',#4198,0.275);
#3588=CYLINDRICAL_SURFACE('',#4201,1.31);
#3589=CYLINDRICAL_SURFACE('',#4223,0.475);
#3590=CYLINDRICAL_SURFACE('',#4228,0.475);
#3591=CYLINDRICAL_SURFACE('',#4232,0.275);
#3592=CYLINDRICAL_SURFACE('',#4234,0.275);
#3593=CYLINDRICAL_SURFACE('',#4236,1.31);
#3594=CYLINDRICAL_SURFACE('',#4245,0.93);
#3595=CYLINDRICAL_SURFACE('',#4250,0.79);
#3596=CYLINDRICAL_SURFACE('',#4252,1.3);
#3597=CYLINDRICAL_SURFACE('',#4258,0.44);
#3598=CYLINDRICAL_SURFACE('',#4261,0.44);
#3599=CYLINDRICAL_SURFACE('',#4264,0.44);
#3600=CYLINDRICAL_SURFACE('',#4267,0.44);
#3601=CYLINDRICAL_SURFACE('',#4273,3.5);
#3602=CYLINDRICAL_SURFACE('',#4275,0.79);
#3603=CYLINDRICAL_SURFACE('',#4278,1.5);
#3604=CYLINDRICAL_SURFACE('',#4283,0.93);
#3605=CYLINDRICAL_SURFACE('',#4288,0.79);
#3606=CYLINDRICAL_SURFACE('',#4290,1.3);
#3607=CYLINDRICAL_SURFACE('',#4296,0.44);
#3608=CYLINDRICAL_SURFACE('',#4299,0.44);
#3609=CYLINDRICAL_SURFACE('',#4302,0.44);
#3610=CYLINDRICAL_SURFACE('',#4305,0.44);
#3611=CYLINDRICAL_SURFACE('',#4311,3.5);
#3612=CYLINDRICAL_SURFACE('',#4313,0.79);
#3613=CYLINDRICAL_SURFACE('',#4316,1.5);
#3614=CYLINDRICAL_SURFACE('',#4321,0.79);
#3615=CYLINDRICAL_SURFACE('',#4324,2.2);
#3616=CYLINDRICAL_SURFACE('',#4344,0.425);
#3617=CYLINDRICAL_SURFACE('',#4352,0.24505);
#3618=CYLINDRICAL_SURFACE('',#4358,0.425);
#3619=CYLINDRICAL_SURFACE('',#4366,0.24505);
#3620=CYLINDRICAL_SURFACE('',#4380,0.79);
#3621=CYLINDRICAL_SURFACE('',#4389,0.79);
#3622=CYLINDRICAL_SURFACE('',#4393,0.93);
#3623=CYLINDRICAL_SURFACE('',#4395,0.93);
#3624=CYLINDRICAL_SURFACE('',#4404,1.2);
#3625=CYLINDRICAL_SURFACE('',#4409,1.45);
#3626=CYLINDRICAL_SURFACE('',#4415,1.45);
#3627=CYLINDRICAL_SURFACE('',#4418,1.2);
#3628=CYLINDRICAL_SURFACE('',#4430,1.065);
#3629=CYLINDRICAL_SURFACE('',#4436,1.065);
#3630=CYLINDRICAL_SURFACE('',#4442,0.79);
#3631=CYLINDRICAL_SURFACE('',#4448,0.65);
#3632=CYLINDRICAL_SURFACE('',#4456,0.3933);
#3633=CYLINDRICAL_SURFACE('',#4470,0.42);
#3634=CYLINDRICAL_SURFACE('',#4473,0.8);
#3635=CYLINDRICAL_SURFACE('',#4486,0.338975);
#3636=ADVANCED_FACE('',(#500),#3570,.F.);
#3637=ADVANCED_FACE('',(#501),#3571,.F.);
#3638=ADVANCED_FACE('',(#502),#3572,.F.);
#3639=ADVANCED_FACE('',(#503),#3573,.F.);
#3640=ADVANCED_FACE('',(#504),#357,.T.);
#3641=ADVANCED_FACE('',(#505),#358,.T.);
#3642=ADVANCED_FACE('',(#506),#359,.T.);
#3643=ADVANCED_FACE('',(#507),#360,.T.);
#3644=ADVANCED_FACE('',(#508,#281,#282,#283,#284),#361,.T.);
#3645=ADVANCED_FACE('',(#509,#285,#286,#287,#288),#362,.F.);
#3646=ADVANCED_FACE('',(#510),#363,.T.);
#3647=ADVANCED_FACE('',(#511),#364,.T.);
#3648=ADVANCED_FACE('',(#512),#365,.T.);
#3649=ADVANCED_FACE('',(#513),#366,.T.);
#3650=ADVANCED_FACE('',(#514),#367,.T.);
#3651=ADVANCED_FACE('',(#515),#368,.F.);
#3652=ADVANCED_FACE('',(#516),#369,.T.);
#3653=ADVANCED_FACE('',(#517),#370,.T.);
#3654=ADVANCED_FACE('',(#518),#371,.T.);
#3655=ADVANCED_FACE('',(#519),#372,.T.);
#3656=ADVANCED_FACE('',(#520),#373,.T.);
#3657=ADVANCED_FACE('',(#521),#374,.F.);
#3658=ADVANCED_FACE('',(#522),#3574,.F.);
#3659=ADVANCED_FACE('',(#523),#375,.T.);
#3660=ADVANCED_FACE('',(#524),#3575,.F.);
#3661=ADVANCED_FACE('',(#525),#376,.T.);
#3662=ADVANCED_FACE('',(#526),#3576,.F.);
#3663=ADVANCED_FACE('',(#527),#3577,.F.);
#3664=ADVANCED_FACE('',(#528),#3578,.F.);
#3665=ADVANCED_FACE('',(#529),#377,.T.);
#3666=ADVANCED_FACE('',(#530,#289),#378,.T.);
#3667=ADVANCED_FACE('',(#531,#290),#379,.T.);
#3668=ADVANCED_FACE('',(#532,#291),#380,.T.);
#3669=ADVANCED_FACE('',(#533),#381,.T.);
#3670=ADVANCED_FACE('',(#534),#382,.T.);
#3671=ADVANCED_FACE('',(#535),#383,.T.);
#3672=ADVANCED_FACE('',(#536),#384,.T.);
#3673=ADVANCED_FACE('',(#537),#385,.T.);
#3674=ADVANCED_FACE('',(#538),#386,.T.);
#3675=ADVANCED_FACE('',(#539,#292),#387,.T.);
#3676=ADVANCED_FACE('',(#540),#388,.T.);
#3677=ADVANCED_FACE('',(#541,#293,#294),#389,.T.);
#3678=ADVANCED_FACE('',(#542),#390,.T.);
#3679=ADVANCED_FACE('',(#543),#391,.F.);
#3680=ADVANCED_FACE('',(#544,#295),#392,.T.);
#3681=ADVANCED_FACE('',(#545),#3579,.F.);
#3682=ADVANCED_FACE('',(#546,#296),#393,.T.);
#3683=ADVANCED_FACE('',(#547),#3580,.F.);
#3684=ADVANCED_FACE('',(#548),#394,.T.);
#3685=ADVANCED_FACE('',(#549),#395,.T.);
#3686=ADVANCED_FACE('',(#550),#3581,.F.);
#3687=ADVANCED_FACE('',(#551),#3582,.F.);
#3688=ADVANCED_FACE('',(#552),#3583,.F.);
#3689=ADVANCED_FACE('',(#553),#396,.T.);
#3690=ADVANCED_FACE('',(#554,#297),#397,.F.);
#3691=ADVANCED_FACE('',(#555),#398,.T.);
#3692=ADVANCED_FACE('',(#556),#399,.T.);
#3693=ADVANCED_FACE('',(#557,#298),#400,.F.);
#3694=ADVANCED_FACE('',(#558),#3584,.F.);
#3695=ADVANCED_FACE('',(#559),#401,.T.);
#3696=ADVANCED_FACE('',(#560),#3585,.F.);
#3697=ADVANCED_FACE('',(#561),#402,.T.);
#3698=ADVANCED_FACE('',(#562),#3586,.F.);
#3699=ADVANCED_FACE('',(#563),#3587,.F.);
#3700=ADVANCED_FACE('',(#564),#3588,.F.);
#3701=ADVANCED_FACE('',(#565),#403,.T.);
#3702=ADVANCED_FACE('',(#566,#299),#404,.T.);
#3703=ADVANCED_FACE('',(#567,#300),#405,.T.);
#3704=ADVANCED_FACE('',(#568,#301),#406,.T.);
#3705=ADVANCED_FACE('',(#569),#407,.T.);
#3706=ADVANCED_FACE('',(#570),#408,.T.);
#3707=ADVANCED_FACE('',(#571),#409,.T.);
#3708=ADVANCED_FACE('',(#572),#410,.T.);
#3709=ADVANCED_FACE('',(#573),#411,.T.);
#3710=ADVANCED_FACE('',(#574),#412,.T.);
#3711=ADVANCED_FACE('',(#575,#302),#413,.T.);
#3712=ADVANCED_FACE('',(#576),#414,.T.);
#3713=ADVANCED_FACE('',(#577,#303,#304),#415,.T.);
#3714=ADVANCED_FACE('',(#578),#416,.T.);
#3715=ADVANCED_FACE('',(#579),#417,.F.);
#3716=ADVANCED_FACE('',(#580,#305),#418,.T.);
#3717=ADVANCED_FACE('',(#581),#3589,.F.);
#3718=ADVANCED_FACE('',(#582,#306),#419,.T.);
#3719=ADVANCED_FACE('',(#583),#3590,.F.);
#3720=ADVANCED_FACE('',(#584),#420,.T.);
#3721=ADVANCED_FACE('',(#585),#421,.T.);
#3722=ADVANCED_FACE('',(#586),#3591,.F.);
#3723=ADVANCED_FACE('',(#587),#3592,.F.);
#3724=ADVANCED_FACE('',(#588),#3593,.F.);
#3725=ADVANCED_FACE('',(#589),#422,.T.);
#3726=ADVANCED_FACE('',(#590,#307),#423,.F.);
#3727=ADVANCED_FACE('',(#591),#424,.T.);
#3728=ADVANCED_FACE('',(#592),#425,.T.);
#3729=ADVANCED_FACE('',(#593,#308),#426,.F.);
#3730=ADVANCED_FACE('',(#594),#3594,.F.);
#3731=ADVANCED_FACE('',(#595,#309),#427,.F.);
#3732=ADVANCED_FACE('',(#596),#3595,.F.);
#3733=ADVANCED_FACE('',(#597),#3596,.T.);
#3734=ADVANCED_FACE('',(#598,#310),#428,.T.);
#3735=ADVANCED_FACE('',(#599,#311),#429,.F.);
#3736=ADVANCED_FACE('',(#600),#3597,.F.);
#3737=ADVANCED_FACE('',(#601),#3598,.F.);
#3738=ADVANCED_FACE('',(#602),#3599,.F.);
#3739=ADVANCED_FACE('',(#603),#3600,.F.);
#3740=ADVANCED_FACE('',(#604,#312,#313,#314,#315,#316),#430,.F.);
#3741=ADVANCED_FACE('',(#605),#3601,.T.);
#3742=ADVANCED_FACE('',(#606),#3602,.F.);
#3743=ADVANCED_FACE('',(#607),#3603,.T.);
#3744=ADVANCED_FACE('',(#608,#317,#318,#319,#320,#321),#431,.T.);
#3745=ADVANCED_FACE('',(#609,#322),#432,.F.);
#3746=ADVANCED_FACE('',(#610),#3604,.F.);
#3747=ADVANCED_FACE('',(#611,#323),#433,.T.);
#3748=ADVANCED_FACE('',(#612),#3605,.F.);
#3749=ADVANCED_FACE('',(#613),#3606,.T.);
#3750=ADVANCED_FACE('',(#614,#324),#434,.T.);
#3751=ADVANCED_FACE('',(#615,#325),#435,.F.);
#3752=ADVANCED_FACE('',(#616),#3607,.F.);
#3753=ADVANCED_FACE('',(#617),#3608,.F.);
#3754=ADVANCED_FACE('',(#618),#3609,.F.);
#3755=ADVANCED_FACE('',(#619),#3610,.F.);
#3756=ADVANCED_FACE('',(#620,#326,#327,#328,#329,#330),#436,.T.);
#3757=ADVANCED_FACE('',(#621),#3611,.T.);
#3758=ADVANCED_FACE('',(#622),#3612,.F.);
#3759=ADVANCED_FACE('',(#623),#3613,.T.);
#3760=ADVANCED_FACE('',(#624,#331),#437,.T.);
#3761=ADVANCED_FACE('',(#625,#332,#333,#334,#335,#336),#438,.F.);
#3762=ADVANCED_FACE('',(#626),#3614,.F.);
#3763=ADVANCED_FACE('',(#627),#3615,.T.);
#3764=ADVANCED_FACE('',(#628,#337),#439,.T.);
#3765=ADVANCED_FACE('',(#629,#338),#440,.F.);
#3766=ADVANCED_FACE('',(#630),#441,.F.);
#3767=ADVANCED_FACE('',(#631),#442,.F.);
#3768=ADVANCED_FACE('',(#632),#443,.F.);
#3769=ADVANCED_FACE('',(#633),#444,.F.);
#3770=ADVANCED_FACE('',(#634),#445,.F.);
#3771=ADVANCED_FACE('',(#635),#446,.F.);
#3772=ADVANCED_FACE('',(#636),#447,.F.);
#3773=ADVANCED_FACE('',(#637),#448,.F.);
#3774=ADVANCED_FACE('',(#638),#449,.F.);
#3775=ADVANCED_FACE('',(#639),#450,.T.);
#3776=ADVANCED_FACE('',(#640),#187,.T.);
#3777=ADVANCED_FACE('',(#641),#3616,.T.);
#3778=ADVANCED_FACE('',(#642),#188,.T.);
#3779=ADVANCED_FACE('',(#643,#339),#451,.T.);
#3780=ADVANCED_FACE('',(#644),#189,.T.);
#3781=ADVANCED_FACE('',(#645),#3617,.T.);
#3782=ADVANCED_FACE('',(#646),#452,.T.);
#3783=ADVANCED_FACE('',(#647),#190,.T.);
#3784=ADVANCED_FACE('',(#648),#3618,.T.);
#3785=ADVANCED_FACE('',(#649),#191,.T.);
#3786=ADVANCED_FACE('',(#650,#340),#453,.T.);
#3787=ADVANCED_FACE('',(#651),#192,.T.);
#3788=ADVANCED_FACE('',(#652),#3619,.T.);
#3789=ADVANCED_FACE('',(#653),#193,.T.);
#3790=ADVANCED_FACE('',(#654),#454,.T.);
#3791=ADVANCED_FACE('',(#655),#455,.F.);
#3792=ADVANCED_FACE('',(#656),#456,.F.);
#3793=ADVANCED_FACE('',(#657),#457,.F.);
#3794=ADVANCED_FACE('',(#658),#458,.F.);
#3795=ADVANCED_FACE('',(#659),#459,.F.);
#3796=ADVANCED_FACE('',(#660),#460,.F.);
#3797=ADVANCED_FACE('',(#661),#461,.F.);
#3798=ADVANCED_FACE('',(#662),#462,.F.);
#3799=ADVANCED_FACE('',(#663),#3620,.F.);
#3800=ADVANCED_FACE('',(#664,#341),#183,.F.);
#3801=ADVANCED_FACE('',(#665),#3621,.F.);
#3802=ADVANCED_FACE('',(#666,#342),#463,.F.);
#3803=ADVANCED_FACE('',(#667),#3622,.F.);
#3804=ADVANCED_FACE('',(#668),#3623,.F.);
#3805=ADVANCED_FACE('',(#669,#343),#464,.F.);
#3806=ADVANCED_FACE('',(#670),#184,.T.);
#3807=ADVANCED_FACE('',(#671),#3624,.T.);
#3808=ADVANCED_FACE('',(#672,#344),#465,.T.);
#3809=ADVANCED_FACE('',(#673),#3625,.T.);
#3810=ADVANCED_FACE('',(#674,#345),#466,.T.);
#3811=ADVANCED_FACE('',(#675,#346),#467,.T.);
#3812=ADVANCED_FACE('',(#676),#3626,.T.);
#3813=ADVANCED_FACE('',(#677,#347),#468,.T.);
#3814=ADVANCED_FACE('',(#678),#3627,.T.);
#3815=ADVANCED_FACE('',(#679,#348),#469,.F.);
#3816=ADVANCED_FACE('',(#680,#349),#470,.T.);
#3817=ADVANCED_FACE('',(#681),#471,.T.);
#3818=ADVANCED_FACE('',(#682),#472,.T.);
#3819=ADVANCED_FACE('',(#683),#473,.T.);
#3820=ADVANCED_FACE('',(#684),#474,.T.);
#3821=ADVANCED_FACE('',(#685),#475,.T.);
#3822=ADVANCED_FACE('',(#686),#476,.T.);
#3823=ADVANCED_FACE('',(#687),#3628,.T.);
#3824=ADVANCED_FACE('',(#688,#350),#477,.T.);
#3825=ADVANCED_FACE('',(#689),#194,.T.);
#3826=ADVANCED_FACE('',(#690),#3629,.T.);
#3827=ADVANCED_FACE('',(#691),#195,.T.);
#3828=ADVANCED_FACE('',(#692,#351),#478,.T.);
#3829=ADVANCED_FACE('',(#693),#3630,.F.);
#3830=ADVANCED_FACE('',(#694),#479,.T.);
#3831=ADVANCED_FACE('',(#695),#196,.T.);
#3832=ADVANCED_FACE('',(#696),#3631,.T.);
#3833=ADVANCED_FACE('',(#697),#197,.T.);
#3834=ADVANCED_FACE('',(#698,#352),#480,.T.);
#3835=ADVANCED_FACE('',(#699),#198,.T.);
#3836=ADVANCED_FACE('',(#700),#3632,.T.);
#3837=ADVANCED_FACE('',(#701),#199,.T.);
#3838=ADVANCED_FACE('',(#702),#481,.T.);
#3839=ADVANCED_FACE('',(#703),#482,.F.);
#3840=ADVANCED_FACE('',(#704),#483,.F.);
#3841=ADVANCED_FACE('',(#705),#484,.F.);
#3842=ADVANCED_FACE('',(#706),#485,.F.);
#3843=ADVANCED_FACE('',(#707),#486,.F.);
#3844=ADVANCED_FACE('',(#708),#487,.F.);
#3845=ADVANCED_FACE('',(#709),#488,.F.);
#3846=ADVANCED_FACE('',(#710),#489,.F.);
#3847=ADVANCED_FACE('',(#711),#3633,.F.);
#3848=ADVANCED_FACE('',(#712),#3634,.T.);
#3849=ADVANCED_FACE('',(#713,#353),#490,.T.);
#3850=ADVANCED_FACE('',(#714,#354),#491,.F.);
#3851=ADVANCED_FACE('',(#715),#200,.T.);
#3852=ADVANCED_FACE('',(#716),#201,.T.);
#3853=ADVANCED_FACE('',(#717),#492,.T.);
#3854=ADVANCED_FACE('',(#718),#493,.T.);
#3855=ADVANCED_FACE('',(#719),#494,.T.);
#3856=ADVANCED_FACE('',(#720),#3635,.F.);
#3857=ADVANCED_FACE('',(#721),#495,.T.);
#3858=ADVANCED_FACE('',(#722),#496,.T.);
#3859=ADVANCED_FACE('',(#723),#497,.T.);
#3860=ADVANCED_FACE('',(#724,#355),#498,.T.);
#3861=ADVANCED_FACE('',(#725,#356),#499,.F.);
#3862=CLOSED_SHELL('',(#3636,#3637,#3638,#3639,#3640,#3641,#3642,#3643,
#3644,#3645));
#3863=CLOSED_SHELL('',(#3646,#3647,#3648,#3649,#3650,#3651));
#3864=CLOSED_SHELL('',(#3652,#3653,#3654,#3655,#3656,#3657));
#3865=CLOSED_SHELL('',(#3658,#3659,#3660,#3661,#3662,#3663,#3664,#3665,
#3666,#3667,#3668,#3669,#3670,#3671,#3672,#3673,#3674,#3675,#3676,#3677,
#3678,#3679));
#3866=CLOSED_SHELL('',(#3680,#3681,#3682,#3683,#3684,#3685,#3686,#3687,
#3688,#3689,#3690,#3691,#3692,#3693));
#3867=CLOSED_SHELL('',(#3694,#3695,#3696,#3697,#3698,#3699,#3700,#3701,
#3702,#3703,#3704,#3705,#3706,#3707,#3708,#3709,#3710,#3711,#3712,#3713,
#3714,#3715));
#3868=CLOSED_SHELL('',(#3716,#3717,#3718,#3719,#3720,#3721,#3722,#3723,
#3724,#3725,#3726,#3727,#3728,#3729));
#3869=CLOSED_SHELL('',(#3730,#3731,#3732,#3733,#3734,#3735));
#3870=CLOSED_SHELL('',(#3736,#3737,#3738,#3739,#3740,#3741,#3742,#3743,
#3744,#3745));
#3871=CLOSED_SHELL('',(#3746,#3747,#3748,#3749,#3750,#3751));
#3872=CLOSED_SHELL('',(#3752,#3753,#3754,#3755,#3756,#3757,#3758,#3759,
#3760,#3761));
#3873=CLOSED_SHELL('',(#3762,#3763,#3764,#3765));
#3874=CLOSED_SHELL('',(#3766,#3767,#3768,#3769,#3770,#3771,#3772,#3773));
#3875=CLOSED_SHELL('',(#3774,#3775,#3776,#3777,#3778,#3779,#3780,#3781));
#3876=CLOSED_SHELL('',(#3782,#3783,#3784,#3785,#3786,#3787,#3788,#3789,
#3790));
#3877=CLOSED_SHELL('',(#3791,#3792,#3793,#3794,#3795,#3796,#3797,#3798));
#3878=CLOSED_SHELL('',(#3799,#3800,#3801,#3802,#3803,#3804,#3805,#3806,
#3807,#3808,#3809,#3810,#3811,#3812,#3813,#3814));
#3879=CLOSED_SHELL('',(#3815,#3816,#3817,#3818,#3819,#3820,#3821,#3822,
#3823,#3824,#3825,#3826,#3827,#3828,#3829));
#3880=CLOSED_SHELL('',(#3830,#3831,#3832,#3833,#3834,#3835,#3836,#3837,
#3838));
#3881=CLOSED_SHELL('',(#3839,#3840,#3841,#3842,#3843,#3844,#3845,#3846));
#3882=CLOSED_SHELL('',(#3847,#3848,#3849,#3850));
#3883=CLOSED_SHELL('',(#3851,#3852,#3853,#3854,#3855,#3856,#3857,#3858,
#3859,#3860,#3861));
#3884=DERIVED_UNIT_ELEMENT(#3922,1.);
#3885=DERIVED_UNIT_ELEMENT(#6880,-3.);
#3886=DERIVED_UNIT_ELEMENT(#3922,1.);
#3887=DERIVED_UNIT_ELEMENT(#6880,-3.);
#3888=DERIVED_UNIT_ELEMENT(#3922,1.);
#3889=DERIVED_UNIT_ELEMENT(#6880,-3.);
#3890=DERIVED_UNIT_ELEMENT(#3922,1.);
#3891=DERIVED_UNIT_ELEMENT(#6880,-3.);
#3892=DERIVED_UNIT_ELEMENT(#3922,1.);
#3893=DERIVED_UNIT_ELEMENT(#6880,-3.);
#3894=DERIVED_UNIT_ELEMENT(#3922,1.);
#3895=DERIVED_UNIT_ELEMENT(#6880,-3.);
#3896=DERIVED_UNIT_ELEMENT(#3922,1.);
#3897=DERIVED_UNIT_ELEMENT(#6880,-3.);
#3898=DERIVED_UNIT_ELEMENT(#3922,1.);
#3899=DERIVED_UNIT_ELEMENT(#6880,-3.);
#3900=DERIVED_UNIT_ELEMENT(#3922,1.);
#3901=DERIVED_UNIT_ELEMENT(#6880,-3.);
#3902=DERIVED_UNIT_ELEMENT(#3922,1.);
#3903=DERIVED_UNIT_ELEMENT(#6880,-3.);
#3904=DERIVED_UNIT_ELEMENT(#3922,1.);
#3905=DERIVED_UNIT_ELEMENT(#6880,-3.);
#3906=DERIVED_UNIT_ELEMENT(#3922,1.);
#3907=DERIVED_UNIT_ELEMENT(#6880,-3.);
#3908=DERIVED_UNIT_ELEMENT(#3922,1.);
#3909=DERIVED_UNIT_ELEMENT(#6880,-3.);
#3910=DERIVED_UNIT_ELEMENT(#3922,1.);
#3911=DERIVED_UNIT_ELEMENT(#6880,-3.);
#3912=DERIVED_UNIT_ELEMENT(#3922,1.);
#3913=DERIVED_UNIT_ELEMENT(#6880,-3.);
#3914=DERIVED_UNIT_ELEMENT(#3922,1.);
#3915=DERIVED_UNIT_ELEMENT(#6880,-3.);
#3916=DERIVED_UNIT_ELEMENT(#3922,1.);
#3917=DERIVED_UNIT_ELEMENT(#6880,-3.);
#3918=DERIVED_UNIT_ELEMENT(#3922,1.);
#3919=DERIVED_UNIT_ELEMENT(#6880,-3.);
#3920=DERIVED_UNIT_ELEMENT(#3922,1.);
#3921=DERIVED_UNIT_ELEMENT(#6880,-3.);
#3922=(
MASS_UNIT()
NAMED_UNIT(*)
SI_UNIT(.KILO.,.GRAM.)
);
#3923=DERIVED_UNIT((#3884,#3885));
#3924=DERIVED_UNIT((#3886,#3887));
#3925=DERIVED_UNIT((#3888,#3889));
#3926=DERIVED_UNIT((#3890,#3891));
#3927=DERIVED_UNIT((#3892,#3893));
#3928=DERIVED_UNIT((#3894,#3895));
#3929=DERIVED_UNIT((#3896,#3897));
#3930=DERIVED_UNIT((#3898,#3899));
#3931=DERIVED_UNIT((#3900,#3901));
#3932=DERIVED_UNIT((#3902,#3903));
#3933=DERIVED_UNIT((#3904,#3905));
#3934=DERIVED_UNIT((#3906,#3907));
#3935=DERIVED_UNIT((#3908,#3909));
#3936=DERIVED_UNIT((#3910,#3911));
#3937=DERIVED_UNIT((#3912,#3913));
#3938=DERIVED_UNIT((#3914,#3915));
#3939=DERIVED_UNIT((#3916,#3917));
#3940=DERIVED_UNIT((#3918,#3919));
#3941=DERIVED_UNIT((#3920,#3921));
#3942=MEASURE_REPRESENTATION_ITEM('density measure',
POSITIVE_RATIO_MEASURE(7850.),#3923);
#3943=MEASURE_REPRESENTATION_ITEM('density measure',
POSITIVE_RATIO_MEASURE(7850.),#3924);
#3944=MEASURE_REPRESENTATION_ITEM('density measure',
POSITIVE_RATIO_MEASURE(7850.),#3925);
#3945=MEASURE_REPRESENTATION_ITEM('density measure',
POSITIVE_RATIO_MEASURE(7850.),#3926);
#3946=MEASURE_REPRESENTATION_ITEM('density measure',
POSITIVE_RATIO_MEASURE(7850.),#3927);
#3947=MEASURE_REPRESENTATION_ITEM('density measure',
POSITIVE_RATIO_MEASURE(7850.),#3928);
#3948=MEASURE_REPRESENTATION_ITEM('density measure',
POSITIVE_RATIO_MEASURE(7850.),#3929);
#3949=MEASURE_REPRESENTATION_ITEM('density measure',
POSITIVE_RATIO_MEASURE(7850.),#3930);
#3950=MEASURE_REPRESENTATION_ITEM('density measure',
POSITIVE_RATIO_MEASURE(7850.),#3931);
#3951=MEASURE_REPRESENTATION_ITEM('density measure',
POSITIVE_RATIO_MEASURE(7850.),#3932);
#3952=MEASURE_REPRESENTATION_ITEM('density measure',
POSITIVE_RATIO_MEASURE(7850.),#3933);
#3953=MEASURE_REPRESENTATION_ITEM('density measure',
POSITIVE_RATIO_MEASURE(7850.),#3934);
#3954=MEASURE_REPRESENTATION_ITEM('density measure',
POSITIVE_RATIO_MEASURE(7850.),#3935);
#3955=MEASURE_REPRESENTATION_ITEM('density measure',
POSITIVE_RATIO_MEASURE(7850.),#3936);
#3956=MEASURE_REPRESENTATION_ITEM('density measure',
POSITIVE_RATIO_MEASURE(7850.),#3937);
#3957=MEASURE_REPRESENTATION_ITEM('density measure',
POSITIVE_RATIO_MEASURE(7850.),#3938);
#3958=MEASURE_REPRESENTATION_ITEM('density measure',
POSITIVE_RATIO_MEASURE(7850.),#3939);
#3959=MEASURE_REPRESENTATION_ITEM('density measure',
POSITIVE_RATIO_MEASURE(7850.),#3940);
#3960=MEASURE_REPRESENTATION_ITEM('density measure',
POSITIVE_RATIO_MEASURE(7850.),#3941);
#3961=PROPERTY_DEFINITION_REPRESENTATION(#4056,#3999);
#3962=PROPERTY_DEFINITION_REPRESENTATION(#4057,#4000);
#3963=PROPERTY_DEFINITION_REPRESENTATION(#4058,#4001);
#3964=PROPERTY_DEFINITION_REPRESENTATION(#4059,#4002);
#3965=PROPERTY_DEFINITION_REPRESENTATION(#4060,#4003);
#3966=PROPERTY_DEFINITION_REPRESENTATION(#4061,#4004);
#3967=PROPERTY_DEFINITION_REPRESENTATION(#4062,#4005);
#3968=PROPERTY_DEFINITION_REPRESENTATION(#4063,#4006);
#3969=PROPERTY_DEFINITION_REPRESENTATION(#4064,#4007);
#3970=PROPERTY_DEFINITION_REPRESENTATION(#4065,#4008);
#3971=PROPERTY_DEFINITION_REPRESENTATION(#4066,#4009);
#3972=PROPERTY_DEFINITION_REPRESENTATION(#4067,#4010);
#3973=PROPERTY_DEFINITION_REPRESENTATION(#4068,#4011);
#3974=PROPERTY_DEFINITION_REPRESENTATION(#4069,#4012);
#3975=PROPERTY_DEFINITION_REPRESENTATION(#4070,#4013);
#3976=PROPERTY_DEFINITION_REPRESENTATION(#4071,#4014);
#3977=PROPERTY_DEFINITION_REPRESENTATION(#4072,#4015);
#3978=PROPERTY_DEFINITION_REPRESENTATION(#4073,#4016);
#3979=PROPERTY_DEFINITION_REPRESENTATION(#4074,#4017);
#3980=PROPERTY_DEFINITION_REPRESENTATION(#4075,#4018);
#3981=PROPERTY_DEFINITION_REPRESENTATION(#4076,#4019);
#3982=PROPERTY_DEFINITION_REPRESENTATION(#4077,#4020);
#3983=PROPERTY_DEFINITION_REPRESENTATION(#4078,#4021);
#3984=PROPERTY_DEFINITION_REPRESENTATION(#4079,#4022);
#3985=PROPERTY_DEFINITION_REPRESENTATION(#4080,#4023);
#3986=PROPERTY_DEFINITION_REPRESENTATION(#4081,#4024);
#3987=PROPERTY_DEFINITION_REPRESENTATION(#4082,#4025);
#3988=PROPERTY_DEFINITION_REPRESENTATION(#4083,#4026);
#3989=PROPERTY_DEFINITION_REPRESENTATION(#4084,#4027);
#3990=PROPERTY_DEFINITION_REPRESENTATION(#4085,#4028);
#3991=PROPERTY_DEFINITION_REPRESENTATION(#4086,#4029);
#3992=PROPERTY_DEFINITION_REPRESENTATION(#4087,#4030);
#3993=PROPERTY_DEFINITION_REPRESENTATION(#4088,#4031);
#3994=PROPERTY_DEFINITION_REPRESENTATION(#4089,#4032);
#3995=PROPERTY_DEFINITION_REPRESENTATION(#4090,#4033);
#3996=PROPERTY_DEFINITION_REPRESENTATION(#4091,#4034);
#3997=PROPERTY_DEFINITION_REPRESENTATION(#4092,#4035);
#3998=PROPERTY_DEFINITION_REPRESENTATION(#4093,#4036);
#3999=REPRESENTATION('material name',(#4037),#6859);
#4000=REPRESENTATION('density',(#3942),#6859);
#4001=REPRESENTATION('material name',(#4038),#6860);
#4002=REPRESENTATION('density',(#3943),#6860);
#4003=REPRESENTATION('material name',(#4039),#6861);
#4004=REPRESENTATION('density',(#3944),#6861);
#4005=REPRESENTATION('material name',(#4040),#6862);
#4006=REPRESENTATION('density',(#3945),#6862);
#4007=REPRESENTATION('material name',(#4041),#6863);
#4008=REPRESENTATION('density',(#3946),#6863);
#4009=REPRESENTATION('material name',(#4042),#6864);
#4010=REPRESENTATION('density',(#3947),#6864);
#4011=REPRESENTATION('material name',(#4043),#6865);
#4012=REPRESENTATION('density',(#3948),#6865);
#4013=REPRESENTATION('material name',(#4044),#6866);
#4014=REPRESENTATION('density',(#3949),#6866);
#4015=REPRESENTATION('material name',(#4045),#6867);
#4016=REPRESENTATION('density',(#3950),#6867);
#4017=REPRESENTATION('material name',(#4046),#6868);
#4018=REPRESENTATION('density',(#3951),#6868);
#4019=REPRESENTATION('material name',(#4047),#6869);
#4020=REPRESENTATION('density',(#3952),#6869);
#4021=REPRESENTATION('material name',(#4048),#6870);
#4022=REPRESENTATION('density',(#3953),#6870);
#4023=REPRESENTATION('material name',(#4049),#6871);
#4024=REPRESENTATION('density',(#3954),#6871);
#4025=REPRESENTATION('material name',(#4050),#6872);
#4026=REPRESENTATION('density',(#3955),#6872);
#4027=REPRESENTATION('material name',(#4051),#6873);
#4028=REPRESENTATION('density',(#3956),#6873);
#4029=REPRESENTATION('material name',(#4052),#6874);
#4030=REPRESENTATION('density',(#3957),#6874);
#4031=REPRESENTATION('material name',(#4053),#6875);
#4032=REPRESENTATION('density',(#3958),#6875);
#4033=REPRESENTATION('material name',(#4054),#6876);
#4034=REPRESENTATION('density',(#3959),#6876);
#4035=REPRESENTATION('material name',(#4055),#6877);
#4036=REPRESENTATION('density',(#3960),#6877);
#4037=DESCRIPTIVE_REPRESENTATION_ITEM('Steel','Steel');
#4038=DESCRIPTIVE_REPRESENTATION_ITEM('Steel','Steel');
#4039=DESCRIPTIVE_REPRESENTATION_ITEM('Steel','Steel');
#4040=DESCRIPTIVE_REPRESENTATION_ITEM('Steel','Steel');
#4041=DESCRIPTIVE_REPRESENTATION_ITEM('Steel','Steel');
#4042=DESCRIPTIVE_REPRESENTATION_ITEM('Steel','Steel');
#4043=DESCRIPTIVE_REPRESENTATION_ITEM('Steel','Steel');
#4044=DESCRIPTIVE_REPRESENTATION_ITEM('Steel','Steel');
#4045=DESCRIPTIVE_REPRESENTATION_ITEM('Steel','Steel');
#4046=DESCRIPTIVE_REPRESENTATION_ITEM('Steel','Steel');
#4047=DESCRIPTIVE_REPRESENTATION_ITEM('Steel','Steel');
#4048=DESCRIPTIVE_REPRESENTATION_ITEM('Steel','Steel');
#4049=DESCRIPTIVE_REPRESENTATION_ITEM('Steel','Steel');
#4050=DESCRIPTIVE_REPRESENTATION_ITEM('Steel','Steel');
#4051=DESCRIPTIVE_REPRESENTATION_ITEM('Steel','Steel');
#4052=DESCRIPTIVE_REPRESENTATION_ITEM('Steel','Steel');
#4053=DESCRIPTIVE_REPRESENTATION_ITEM('Steel','Steel');
#4054=DESCRIPTIVE_REPRESENTATION_ITEM('Steel','Steel');
#4055=DESCRIPTIVE_REPRESENTATION_ITEM('Steel','Steel');
#4056=PROPERTY_DEFINITION('material property','material name',#6985);
#4057=PROPERTY_DEFINITION('material property','density of part',#6985);
#4058=PROPERTY_DEFINITION('material property','material name',#6986);
#4059=PROPERTY_DEFINITION('material property','density of part',#6986);
#4060=PROPERTY_DEFINITION('material property','material name',#6987);
#4061=PROPERTY_DEFINITION('material property','density of part',#6987);
#4062=PROPERTY_DEFINITION('material property','material name',#6988);
#4063=PROPERTY_DEFINITION('material property','density of part',#6988);
#4064=PROPERTY_DEFINITION('material property','material name',#6989);
#4065=PROPERTY_DEFINITION('material property','density of part',#6989);
#4066=PROPERTY_DEFINITION('material property','material name',#6990);
#4067=PROPERTY_DEFINITION('material property','density of part',#6990);
#4068=PROPERTY_DEFINITION('material property','material name',#6991);
#4069=PROPERTY_DEFINITION('material property','density of part',#6991);
#4070=PROPERTY_DEFINITION('material property','material name',#6992);
#4071=PROPERTY_DEFINITION('material property','density of part',#6992);
#4072=PROPERTY_DEFINITION('material property','material name',#6993);
#4073=PROPERTY_DEFINITION('material property','density of part',#6993);
#4074=PROPERTY_DEFINITION('material property','material name',#6994);
#4075=PROPERTY_DEFINITION('material property','density of part',#6994);
#4076=PROPERTY_DEFINITION('material property','material name',#6995);
#4077=PROPERTY_DEFINITION('material property','density of part',#6995);
#4078=PROPERTY_DEFINITION('material property','material name',#6996);
#4079=PROPERTY_DEFINITION('material property','density of part',#6996);
#4080=PROPERTY_DEFINITION('material property','material name',#6997);
#4081=PROPERTY_DEFINITION('material property','density of part',#6997);
#4082=PROPERTY_DEFINITION('material property','material name',#6998);
#4083=PROPERTY_DEFINITION('material property','density of part',#6998);
#4084=PROPERTY_DEFINITION('material property','material name',#6999);
#4085=PROPERTY_DEFINITION('material property','density of part',#6999);
#4086=PROPERTY_DEFINITION('material property','material name',#7000);
#4087=PROPERTY_DEFINITION('material property','density of part',#7000);
#4088=PROPERTY_DEFINITION('material property','material name',#7001);
#4089=PROPERTY_DEFINITION('material property','density of part',#7001);
#4090=PROPERTY_DEFINITION('material property','material name',#7002);
#4091=PROPERTY_DEFINITION('material property','density of part',#7002);
#4092=PROPERTY_DEFINITION('material property','material name',#7003);
#4093=PROPERTY_DEFINITION('material property','density of part',#7003);
#4094=AXIS2_PLACEMENT_3D('',#5729,#4534,#4535);
#4095=AXIS2_PLACEMENT_3D('',#5730,#4536,#4537);
#4096=AXIS2_PLACEMENT_3D('',#5731,#4538,#4539);
#4097=AXIS2_PLACEMENT_3D('',#5733,#4540,#4541);
#4098=AXIS2_PLACEMENT_3D('',#5736,#4543,#4544);
#4099=AXIS2_PLACEMENT_3D('',#5737,#4545,#4546);
#4100=AXIS2_PLACEMENT_3D('',#5739,#4547,#4548);
#4101=AXIS2_PLACEMENT_3D('',#5742,#4550,#4551);
#4102=AXIS2_PLACEMENT_3D('',#5743,#4552,#4553);
#4103=AXIS2_PLACEMENT_3D('',#5745,#4554,#4555);
#4104=AXIS2_PLACEMENT_3D('',#5748,#4557,#4558);
#4105=AXIS2_PLACEMENT_3D('',#5749,#4559,#4560);
#4106=AXIS2_PLACEMENT_3D('',#5751,#4561,#4562);
#4107=AXIS2_PLACEMENT_3D('',#5754,#4564,#4565);
#4108=AXIS2_PLACEMENT_3D('',#5755,#4566,#4567);
#4109=AXIS2_PLACEMENT_3D('',#5764,#4572,#4573);
#4110=AXIS2_PLACEMENT_3D('',#5770,#4577,#4578);
#4111=AXIS2_PLACEMENT_3D('',#5776,#4582,#4583);
#4112=AXIS2_PLACEMENT_3D('',#5779,#4586,#4587);
#4113=AXIS2_PLACEMENT_3D('',#5780,#4588,#4589);
#4114=AXIS2_PLACEMENT_3D('',#5781,#4590,#4591);
#4115=AXIS2_PLACEMENT_3D('',#5782,#4592,#4593);
#4116=AXIS2_PLACEMENT_3D('',#5791,#4598,#4599);
#4117=AXIS2_PLACEMENT_3D('',#5797,#4603,#4604);
#4118=AXIS2_PLACEMENT_3D('',#5803,#4608,#4609);
#4119=AXIS2_PLACEMENT_3D('',#5806,#4612,#4613);
#4120=AXIS2_PLACEMENT_3D('',#5807,#4614,#4615);
#4121=AXIS2_PLACEMENT_3D('',#5808,#4616,#4617);
#4122=AXIS2_PLACEMENT_3D('',#5809,#4618,#4619);
#4123=AXIS2_PLACEMENT_3D('',#5818,#4624,#4625);
#4124=AXIS2_PLACEMENT_3D('',#5824,#4629,#4630);
#4125=AXIS2_PLACEMENT_3D('',#5830,#4634,#4635);
#4126=AXIS2_PLACEMENT_3D('',#5833,#4638,#4639);
#4127=AXIS2_PLACEMENT_3D('',#5834,#4640,#4641);
#4128=AXIS2_PLACEMENT_3D('',#5835,#4642,#4643);
#4129=AXIS2_PLACEMENT_3D('',#5836,#4644,#4645);
#4130=AXIS2_PLACEMENT_3D('',#5838,#4646,#4647);
#4131=AXIS2_PLACEMENT_3D('',#5841,#4649,#4650);
#4132=AXIS2_PLACEMENT_3D('',#5842,#4651,#4652);
#4133=AXIS2_PLACEMENT_3D('',#5843,#4653,#4654);
#4134=AXIS2_PLACEMENT_3D('',#5845,#4655,#4656);
#4135=AXIS2_PLACEMENT_3D('',#5848,#4658,#4659);
#4136=AXIS2_PLACEMENT_3D('',#5849,#4660,#4661);
#4137=AXIS2_PLACEMENT_3D('',#5850,#4662,#4663);
#4138=AXIS2_PLACEMENT_3D('',#5852,#4664,#4665);
#4139=AXIS2_PLACEMENT_3D('',#5855,#4667,#4668);
#4140=AXIS2_PLACEMENT_3D('',#5856,#4669,#4670);
#4141=AXIS2_PLACEMENT_3D('',#5858,#4671,#4672);
#4142=AXIS2_PLACEMENT_3D('',#5861,#4674,#4675);
#4143=AXIS2_PLACEMENT_3D('',#5862,#4676,#4677);
#4144=AXIS2_PLACEMENT_3D('',#5867,#4679,#4680);
#4145=AXIS2_PLACEMENT_3D('',#5870,#4682,#4683);
#4146=AXIS2_PLACEMENT_3D('',#5871,#4684,#4685);
#4147=AXIS2_PLACEMENT_3D('',#5897,#4699,#4700);
#4148=AXIS2_PLACEMENT_3D('',#5901,#4703,#4704);
#4149=AXIS2_PLACEMENT_3D('',#5905,#4707,#4708);
#4150=AXIS2_PLACEMENT_3D('',#5911,#4712,#4713);
#4151=AXIS2_PLACEMENT_3D('',#5915,#4716,#4717);
#4152=AXIS2_PLACEMENT_3D('',#5919,#4720,#4721);
#4153=AXIS2_PLACEMENT_3D('',#5921,#4723,#4724);
#4154=AXIS2_PLACEMENT_3D('',#5925,#4727,#4728);
#4155=AXIS2_PLACEMENT_3D('',#5929,#4731,#4732);
#4156=AXIS2_PLACEMENT_3D('',#5933,#4735,#4736);
#4157=AXIS2_PLACEMENT_3D('',#5937,#4739,#4740);
#4158=AXIS2_PLACEMENT_3D('',#5941,#4743,#4744);
#4159=AXIS2_PLACEMENT_3D('',#5945,#4747,#4748);
#4160=AXIS2_PLACEMENT_3D('',#5947,#4750,#4751);
#4161=AXIS2_PLACEMENT_3D('',#5948,#4752,#4753);
#4162=AXIS2_PLACEMENT_3D('',#5949,#4754,#4755);
#4163=AXIS2_PLACEMENT_3D('',#5953,#4757,#4758);
#4164=AXIS2_PLACEMENT_3D('',#5955,#4759,#4760);
#4165=AXIS2_PLACEMENT_3D('',#5956,#4761,#4762);
#4166=AXIS2_PLACEMENT_3D('',#5960,#4764,#4765);
#4167=AXIS2_PLACEMENT_3D('',#5962,#4767,#4768);
#4168=AXIS2_PLACEMENT_3D('',#5966,#4770,#4771);
#4169=AXIS2_PLACEMENT_3D('',#5968,#4772,#4773);
#4170=AXIS2_PLACEMENT_3D('',#5969,#4774,#4775);
#4171=AXIS2_PLACEMENT_3D('',#5973,#4777,#4778);
#4172=AXIS2_PLACEMENT_3D('',#5975,#4780,#4781);
#4173=AXIS2_PLACEMENT_3D('',#5985,#4787,#4788);
#4174=AXIS2_PLACEMENT_3D('',#5995,#4794,#4795);
#4175=AXIS2_PLACEMENT_3D('',#5997,#4796,#4797);
#4176=AXIS2_PLACEMENT_3D('',#5999,#4799,#4800);
#4177=AXIS2_PLACEMENT_3D('',#6001,#4801,#4802);
#4178=AXIS2_PLACEMENT_3D('',#6003,#4804,#4805);
#4179=AXIS2_PLACEMENT_3D('',#6006,#4806,#4807);
#4180=AXIS2_PLACEMENT_3D('',#6010,#4809,#4810);
#4181=AXIS2_PLACEMENT_3D('',#6012,#4812,#4813);
#4182=AXIS2_PLACEMENT_3D('',#6016,#4817,#4818);
#4183=AXIS2_PLACEMENT_3D('',#6018,#4820,#4821);
#4184=AXIS2_PLACEMENT_3D('',#6021,#4824,#4825);
#4185=AXIS2_PLACEMENT_3D('',#6022,#4826,#4827);
#4186=AXIS2_PLACEMENT_3D('',#6023,#4828,#4829);
#4187=AXIS2_PLACEMENT_3D('',#6024,#4830,#4831);
#4188=AXIS2_PLACEMENT_3D('',#6026,#4832,#4833);
#4189=AXIS2_PLACEMENT_3D('',#6029,#4835,#4836);
#4190=AXIS2_PLACEMENT_3D('',#6030,#4837,#4838);
#4191=AXIS2_PLACEMENT_3D('',#6031,#4839,#4840);
#4192=AXIS2_PLACEMENT_3D('',#6033,#4841,#4842);
#4193=AXIS2_PLACEMENT_3D('',#6036,#4844,#4845);
#4194=AXIS2_PLACEMENT_3D('',#6037,#4846,#4847);
#4195=AXIS2_PLACEMENT_3D('',#6038,#4848,#4849);
#4196=AXIS2_PLACEMENT_3D('',#6040,#4850,#4851);
#4197=AXIS2_PLACEMENT_3D('',#6043,#4853,#4854);
#4198=AXIS2_PLACEMENT_3D('',#6044,#4855,#4856);
#4199=AXIS2_PLACEMENT_3D('',#6046,#4857,#4858);
#4200=AXIS2_PLACEMENT_3D('',#6049,#4860,#4861);
#4201=AXIS2_PLACEMENT_3D('',#6050,#4862,#4863);
#4202=AXIS2_PLACEMENT_3D('',#6055,#4865,#4866);
#4203=AXIS2_PLACEMENT_3D('',#6058,#4868,#4869);
#4204=AXIS2_PLACEMENT_3D('',#6059,#4870,#4871);
#4205=AXIS2_PLACEMENT_3D('',#6085,#4885,#4886);
#4206=AXIS2_PLACEMENT_3D('',#6089,#4889,#4890);
#4207=AXIS2_PLACEMENT_3D('',#6093,#4893,#4894);
#4208=AXIS2_PLACEMENT_3D('',#6099,#4898,#4899);
#4209=AXIS2_PLACEMENT_3D('',#6103,#4902,#4903);
#4210=AXIS2_PLACEMENT_3D('',#6107,#4906,#4907);
#4211=AXIS2_PLACEMENT_3D('',#6109,#4909,#4910);
#4212=AXIS2_PLACEMENT_3D('',#6113,#4913,#4914);
#4213=AXIS2_PLACEMENT_3D('',#6117,#4917,#4918);
#4214=AXIS2_PLACEMENT_3D('',#6121,#4921,#4922);
#4215=AXIS2_PLACEMENT_3D('',#6125,#4925,#4926);
#4216=AXIS2_PLACEMENT_3D('',#6129,#4929,#4930);
#4217=AXIS2_PLACEMENT_3D('',#6133,#4933,#4934);
#4218=AXIS2_PLACEMENT_3D('',#6135,#4936,#4937);
#4219=AXIS2_PLACEMENT_3D('',#6136,#4938,#4939);
#4220=AXIS2_PLACEMENT_3D('',#6137,#4940,#4941);
#4221=AXIS2_PLACEMENT_3D('',#6141,#4943,#4944);
#4222=AXIS2_PLACEMENT_3D('',#6143,#4945,#4946);
#4223=AXIS2_PLACEMENT_3D('',#6144,#4947,#4948);
#4224=AXIS2_PLACEMENT_3D('',#6148,#4950,#4951);
#4225=AXIS2_PLACEMENT_3D('',#6150,#4953,#4954);
#4226=AXIS2_PLACEMENT_3D('',#6154,#4956,#4957);
#4227=AXIS2_PLACEMENT_3D('',#6156,#4958,#4959);
#4228=AXIS2_PLACEMENT_3D('',#6157,#4960,#4961);
#4229=AXIS2_PLACEMENT_3D('',#6161,#4963,#4964);
#4230=AXIS2_PLACEMENT_3D('',#6163,#4966,#4967);
#4231=AXIS2_PLACEMENT_3D('',#6173,#4973,#4974);
#4232=AXIS2_PLACEMENT_3D('',#6183,#4980,#4981);
#4233=AXIS2_PLACEMENT_3D('',#6185,#4982,#4983);
#4234=AXIS2_PLACEMENT_3D('',#6187,#4985,#4986);
#4235=AXIS2_PLACEMENT_3D('',#6189,#4987,#4988);
#4236=AXIS2_PLACEMENT_3D('',#6191,#4990,#4991);
#4237=AXIS2_PLACEMENT_3D('',#6194,#4992,#4993);
#4238=AXIS2_PLACEMENT_3D('',#6198,#4995,#4996);
#4239=AXIS2_PLACEMENT_3D('',#6200,#4998,#4999);
#4240=AXIS2_PLACEMENT_3D('',#6204,#5003,#5004);
#4241=AXIS2_PLACEMENT_3D('',#6206,#5006,#5007);
#4242=AXIS2_PLACEMENT_3D('',#6209,#5010,#5011);
#4243=AXIS2_PLACEMENT_3D('',#6210,#5012,#5013);
#4244=AXIS2_PLACEMENT_3D('',#6211,#5014,#5015);
#4245=AXIS2_PLACEMENT_3D('',#6212,#5016,#5017);
#4246=AXIS2_PLACEMENT_3D('',#6214,#5018,#5019);
#4247=AXIS2_PLACEMENT_3D('',#6217,#5021,#5022);
#4248=AXIS2_PLACEMENT_3D('',#6218,#5023,#5024);
#4249=AXIS2_PLACEMENT_3D('',#6220,#5025,#5026);
#4250=AXIS2_PLACEMENT_3D('',#6221,#5027,#5028);
#4251=AXIS2_PLACEMENT_3D('',#6223,#5029,#5030);
#4252=AXIS2_PLACEMENT_3D('',#6225,#5032,#5033);
#4253=AXIS2_PLACEMENT_3D('',#6227,#5034,#5035);
#4254=AXIS2_PLACEMENT_3D('',#6230,#5037,#5038);
#4255=AXIS2_PLACEMENT_3D('',#6231,#5039,#5040);
#4256=AXIS2_PLACEMENT_3D('',#6232,#5041,#5042);
#4257=AXIS2_PLACEMENT_3D('',#6233,#5043,#5044);
#4258=AXIS2_PLACEMENT_3D('',#6234,#5045,#5046);
#4259=AXIS2_PLACEMENT_3D('',#6236,#5047,#5048);
#4260=AXIS2_PLACEMENT_3D('',#6239,#5050,#5051);
#4261=AXIS2_PLACEMENT_3D('',#6240,#5052,#5053);
#4262=AXIS2_PLACEMENT_3D('',#6242,#5054,#5055);
#4263=AXIS2_PLACEMENT_3D('',#6245,#5057,#5058);
#4264=AXIS2_PLACEMENT_3D('',#6246,#5059,#5060);
#4265=AXIS2_PLACEMENT_3D('',#6248,#5061,#5062);
#4266=AXIS2_PLACEMENT_3D('',#6251,#5064,#5065);
#4267=AXIS2_PLACEMENT_3D('',#6252,#5066,#5067);
#4268=AXIS2_PLACEMENT_3D('',#6254,#5068,#5069);
#4269=AXIS2_PLACEMENT_3D('',#6257,#5071,#5072);
#4270=AXIS2_PLACEMENT_3D('',#6258,#5073,#5074);
#4271=AXIS2_PLACEMENT_3D('',#6260,#5075,#5076);
#4272=AXIS2_PLACEMENT_3D('',#6262,#5077,#5078);
#4273=AXIS2_PLACEMENT_3D('',#6263,#5079,#5080);
#4274=AXIS2_PLACEMENT_3D('',#6265,#5081,#5082);
#4275=AXIS2_PLACEMENT_3D('',#6267,#5084,#5085);
#4276=AXIS2_PLACEMENT_3D('',#6269,#5086,#5087);
#4277=AXIS2_PLACEMENT_3D('',#6272,#5089,#5090);
#4278=AXIS2_PLACEMENT_3D('',#6273,#5091,#5092);
#4279=AXIS2_PLACEMENT_3D('',#6276,#5094,#5095);
#4280=AXIS2_PLACEMENT_3D('',#6277,#5096,#5097);
#4281=AXIS2_PLACEMENT_3D('',#6278,#5098,#5099);
#4282=AXIS2_PLACEMENT_3D('',#6279,#5100,#5101);
#4283=AXIS2_PLACEMENT_3D('',#6280,#5102,#5103);
#4284=AXIS2_PLACEMENT_3D('',#6282,#5104,#5105);
#4285=AXIS2_PLACEMENT_3D('',#6285,#5107,#5108);
#4286=AXIS2_PLACEMENT_3D('',#6286,#5109,#5110);
#4287=AXIS2_PLACEMENT_3D('',#6288,#5111,#5112);
#4288=AXIS2_PLACEMENT_3D('',#6289,#5113,#5114);
#4289=AXIS2_PLACEMENT_3D('',#6292,#5116,#5117);
#4290=AXIS2_PLACEMENT_3D('',#6293,#5118,#5119);
#4291=AXIS2_PLACEMENT_3D('',#6295,#5120,#5121);
#4292=AXIS2_PLACEMENT_3D('',#6298,#5123,#5124);
#4293=AXIS2_PLACEMENT_3D('',#6299,#5125,#5126);
#4294=AXIS2_PLACEMENT_3D('',#6300,#5127,#5128);
#4295=AXIS2_PLACEMENT_3D('',#6301,#5129,#5130);
#4296=AXIS2_PLACEMENT_3D('',#6302,#5131,#5132);
#4297=AXIS2_PLACEMENT_3D('',#6304,#5133,#5134);
#4298=AXIS2_PLACEMENT_3D('',#6307,#5136,#5137);
#4299=AXIS2_PLACEMENT_3D('',#6308,#5138,#5139);
#4300=AXIS2_PLACEMENT_3D('',#6310,#5140,#5141);
#4301=AXIS2_PLACEMENT_3D('',#6313,#5143,#5144);
#4302=AXIS2_PLACEMENT_3D('',#6314,#5145,#5146);
#4303=AXIS2_PLACEMENT_3D('',#6316,#5147,#5148);
#4304=AXIS2_PLACEMENT_3D('',#6319,#5150,#5151);
#4305=AXIS2_PLACEMENT_3D('',#6320,#5152,#5153);
#4306=AXIS2_PLACEMENT_3D('',#6322,#5154,#5155);
#4307=AXIS2_PLACEMENT_3D('',#6325,#5157,#5158);
#4308=AXIS2_PLACEMENT_3D('',#6326,#5159,#5160);
#4309=AXIS2_PLACEMENT_3D('',#6328,#5161,#5162);
#4310=AXIS2_PLACEMENT_3D('',#6330,#5163,#5164);
#4311=AXIS2_PLACEMENT_3D('',#6331,#5165,#5166);
#4312=AXIS2_PLACEMENT_3D('',#6334,#5168,#5169);
#4313=AXIS2_PLACEMENT_3D('',#6335,#5170,#5171);
#4314=AXIS2_PLACEMENT_3D('',#6337,#5172,#5173);
#4315=AXIS2_PLACEMENT_3D('',#6340,#5175,#5176);
#4316=AXIS2_PLACEMENT_3D('',#6341,#5177,#5178);
#4317=AXIS2_PLACEMENT_3D('',#6343,#5179,#5180);
#4318=AXIS2_PLACEMENT_3D('',#6345,#5182,#5183);
#4319=AXIS2_PLACEMENT_3D('',#6346,#5184,#5185);
#4320=AXIS2_PLACEMENT_3D('',#6347,#5186,#5187);
#4321=AXIS2_PLACEMENT_3D('',#6348,#5188,#5189);
#4322=AXIS2_PLACEMENT_3D('',#6350,#5190,#5191);
#4323=AXIS2_PLACEMENT_3D('',#6353,#5193,#5194);
#4324=AXIS2_PLACEMENT_3D('',#6354,#5195,#5196);
#4325=AXIS2_PLACEMENT_3D('',#6356,#5197,#5198);
#4326=AXIS2_PLACEMENT_3D('',#6359,#5200,#5201);
#4327=AXIS2_PLACEMENT_3D('',#6360,#5202,#5203);
#4328=AXIS2_PLACEMENT_3D('',#6361,#5204,#5205);
#4329=AXIS2_PLACEMENT_3D('',#6362,#5206,#5207);
#4330=AXIS2_PLACEMENT_3D('',#6363,#5208,#5209);
#4331=AXIS2_PLACEMENT_3D('',#6372,#5214,#5215);
#4332=AXIS2_PLACEMENT_3D('',#6378,#5219,#5220);
#4333=AXIS2_PLACEMENT_3D('',#6384,#5224,#5225);
#4334=AXIS2_PLACEMENT_3D('',#6390,#5229,#5230);
#4335=AXIS2_PLACEMENT_3D('',#6396,#5234,#5235);
#4336=AXIS2_PLACEMENT_3D('',#6399,#5238,#5239);
#4337=AXIS2_PLACEMENT_3D('',#6400,#5240,#5241);
#4338=AXIS2_PLACEMENT_3D('',#6401,#5242,#5243);
#4339=AXIS2_PLACEMENT_3D('',#6403,#5244,#5245);
#4340=AXIS2_PLACEMENT_3D('',#6404,#5246,#5247);
#4341=AXIS2_PLACEMENT_3D('',#6406,#5248,#5249);
#4342=AXIS2_PLACEMENT_3D('',#6407,#5250,#5251);
#4343=AXIS2_PLACEMENT_3D('',#6409,#5252,#5253);
#4344=AXIS2_PLACEMENT_3D('',#6411,#5255,#5256);
#4345=AXIS2_PLACEMENT_3D('',#6413,#5257,#5258);
#4346=AXIS2_PLACEMENT_3D('',#6415,#5260,#5261);
#4347=AXIS2_PLACEMENT_3D('',#6417,#5262,#5263);
#4348=AXIS2_PLACEMENT_3D('',#6419,#5265,#5266);
#4349=AXIS2_PLACEMENT_3D('',#6421,#5267,#5268);
#4350=AXIS2_PLACEMENT_3D('',#6422,#5269,#5270);
#4351=AXIS2_PLACEMENT_3D('',#6424,#5271,#5272);
#4352=AXIS2_PLACEMENT_3D('',#6426,#5274,#5275);
#4353=AXIS2_PLACEMENT_3D('',#6428,#5277,#5278);
#4354=AXIS2_PLACEMENT_3D('',#6429,#5279,#5280);
#4355=AXIS2_PLACEMENT_3D('',#6431,#5281,#5282);
#4356=AXIS2_PLACEMENT_3D('',#6432,#5283,#5284);
#4357=AXIS2_PLACEMENT_3D('',#6434,#5285,#5286);
#4358=AXIS2_PLACEMENT_3D('',#6436,#5288,#5289);
#4359=AXIS2_PLACEMENT_3D('',#6438,#5290,#5291);
#4360=AXIS2_PLACEMENT_3D('',#6440,#5293,#5294);
#4361=AXIS2_PLACEMENT_3D('',#6442,#5295,#5296);
#4362=AXIS2_PLACEMENT_3D('',#6444,#5298,#5299);
#4363=AXIS2_PLACEMENT_3D('',#6446,#5300,#5301);
#4364=AXIS2_PLACEMENT_3D('',#6447,#5302,#5303);
#4365=AXIS2_PLACEMENT_3D('',#6449,#5304,#5305);
#4366=AXIS2_PLACEMENT_3D('',#6451,#5307,#5308);
#4367=AXIS2_PLACEMENT_3D('',#6453,#5309,#5310);
#4368=AXIS2_PLACEMENT_3D('',#6455,#5312,#5313);
#4369=AXIS2_PLACEMENT_3D('',#6457,#5314,#5315);
#4370=AXIS2_PLACEMENT_3D('',#6459,#5317,#5318);
#4371=AXIS2_PLACEMENT_3D('',#6460,#5319,#5320);
#4372=AXIS2_PLACEMENT_3D('',#6469,#5325,#5326);
#4373=AXIS2_PLACEMENT_3D('',#6475,#5330,#5331);
#4374=AXIS2_PLACEMENT_3D('',#6481,#5335,#5336);
#4375=AXIS2_PLACEMENT_3D('',#6487,#5340,#5341);
#4376=AXIS2_PLACEMENT_3D('',#6493,#5345,#5346);
#4377=AXIS2_PLACEMENT_3D('',#6496,#5349,#5350);
#4378=AXIS2_PLACEMENT_3D('',#6497,#5351,#5352);
#4379=AXIS2_PLACEMENT_3D('',#6498,#5353,#5354);
#4380=AXIS2_PLACEMENT_3D('',#6499,#5355,#5356);
#4381=AXIS2_PLACEMENT_3D('',#6502,#5357,#5358);
#4382=AXIS2_PLACEMENT_3D('',#6504,#5359,#5360);
#4383=AXIS2_PLACEMENT_3D('',#6507,#5362,#5363);
#4384=AXIS2_PLACEMENT_3D('',#6508,#5364,#5365);
#4385=AXIS2_PLACEMENT_3D('',#6509,#5366,#5367);
#4386=AXIS2_PLACEMENT_3D('',#6512,#5368,#5369);
#4387=AXIS2_PLACEMENT_3D('',#6514,#5370,#5371);
#4388=AXIS2_PLACEMENT_3D('',#6515,#5372,#5373);
#4389=AXIS2_PLACEMENT_3D('',#6516,#5374,#5375);
#4390=AXIS2_PLACEMENT_3D('',#6519,#5377,#5378);
#4391=AXIS2_PLACEMENT_3D('',#6520,#5379,#5380);
#4392=AXIS2_PLACEMENT_3D('',#6522,#5381,#5382);
#4393=AXIS2_PLACEMENT_3D('',#6523,#5383,#5384);
#4394=AXIS2_PLACEMENT_3D('',#6525,#5385,#5386);
#4395=AXIS2_PLACEMENT_3D('',#6527,#5388,#5389);
#4396=AXIS2_PLACEMENT_3D('',#6529,#5390,#5391);
#4397=AXIS2_PLACEMENT_3D('',#6532,#5393,#5394);
#4398=AXIS2_PLACEMENT_3D('',#6533,#5395,#5396);
#4399=AXIS2_PLACEMENT_3D('',#6534,#5397,#5398);
#4400=AXIS2_PLACEMENT_3D('',#6537,#5399,#5400);
#4401=AXIS2_PLACEMENT_3D('',#6539,#5401,#5402);
#4402=AXIS2_PLACEMENT_3D('',#6541,#5403,#5404);
#4403=AXIS2_PLACEMENT_3D('',#6542,#5405,#5406);
#4404=AXIS2_PLACEMENT_3D('',#6543,#5407,#5408);
#4405=AXIS2_PLACEMENT_3D('',#6544,#5409,#5410);
#4406=AXIS2_PLACEMENT_3D('',#6547,#5412,#5413);
#4407=AXIS2_PLACEMENT_3D('',#6548,#5414,#5415);
#4408=AXIS2_PLACEMENT_3D('',#6550,#5416,#5417);
#4409=AXIS2_PLACEMENT_3D('',#6551,#5418,#5419);
#4410=AXIS2_PLACEMENT_3D('',#6553,#5420,#5421);
#4411=AXIS2_PLACEMENT_3D('',#6555,#5423,#5424);
#4412=AXIS2_PLACEMENT_3D('',#6556,#5425,#5426);
#4413=AXIS2_PLACEMENT_3D('',#6558,#5427,#5428);
#4414=AXIS2_PLACEMENT_3D('',#6560,#5429,#5430);
#4415=AXIS2_PLACEMENT_3D('',#6561,#5431,#5432);
#4416=AXIS2_PLACEMENT_3D('',#6563,#5433,#5434);
#4417=AXIS2_PLACEMENT_3D('',#6565,#5436,#5437);
#4418=AXIS2_PLACEMENT_3D('',#6566,#5438,#5439);
#4419=AXIS2_PLACEMENT_3D('',#6568,#5441,#5442);
#4420=AXIS2_PLACEMENT_3D('',#6569,#5443,#5444);
#4421=AXIS2_PLACEMENT_3D('',#6583,#5451,#5452);
#4422=AXIS2_PLACEMENT_3D('',#6584,#5453,#5454);
#4423=AXIS2_PLACEMENT_3D('',#6598,#5461,#5462);
#4424=AXIS2_PLACEMENT_3D('',#6599,#5463,#5464);
#4425=AXIS2_PLACEMENT_3D('',#6602,#5467,#5468);
#4426=AXIS2_PLACEMENT_3D('',#6604,#5470,#5471);
#4427=AXIS2_PLACEMENT_3D('',#6606,#5473,#5474);
#4428=AXIS2_PLACEMENT_3D('',#6608,#5476,#5477);
#4429=AXIS2_PLACEMENT_3D('',#6610,#5479,#5480);
#4430=AXIS2_PLACEMENT_3D('',#6611,#5481,#5482);
#4431=AXIS2_PLACEMENT_3D('',#6614,#5484,#5485);
#4432=AXIS2_PLACEMENT_3D('',#6615,#5486,#5487);
#4433=AXIS2_PLACEMENT_3D('',#6617,#5488,#5489);
#4434=AXIS2_PLACEMENT_3D('',#6619,#5490,#5491);
#4435=AXIS2_PLACEMENT_3D('',#6620,#5492,#5493);
#4436=AXIS2_PLACEMENT_3D('',#6622,#5495,#5496);
#4437=AXIS2_PLACEMENT_3D('',#6624,#5497,#5498);
#4438=AXIS2_PLACEMENT_3D('',#6626,#5500,#5501);
#4439=AXIS2_PLACEMENT_3D('',#6628,#5502,#5503);
#4440=AXIS2_PLACEMENT_3D('',#6630,#5505,#5506);
#4441=AXIS2_PLACEMENT_3D('',#6632,#5507,#5508);
#4442=AXIS2_PLACEMENT_3D('',#6633,#5509,#5510);
#4443=AXIS2_PLACEMENT_3D('',#6635,#5512,#5513);
#4444=AXIS2_PLACEMENT_3D('',#6636,#5514,#5515);
#4445=AXIS2_PLACEMENT_3D('',#6638,#5516,#5517);
#4446=AXIS2_PLACEMENT_3D('',#6639,#5518,#5519);
#4447=AXIS2_PLACEMENT_3D('',#6641,#5520,#5521);
#4448=AXIS2_PLACEMENT_3D('',#6643,#5523,#5524);
#4449=AXIS2_PLACEMENT_3D('',#6645,#5525,#5526);
#4450=AXIS2_PLACEMENT_3D('',#6647,#5528,#5529);
#4451=AXIS2_PLACEMENT_3D('',#6649,#5530,#5531);
#4452=AXIS2_PLACEMENT_3D('',#6651,#5533,#5534);
#4453=AXIS2_PLACEMENT_3D('',#6653,#5535,#5536);
#4454=AXIS2_PLACEMENT_3D('',#6654,#5537,#5538);
#4455=AXIS2_PLACEMENT_3D('',#6656,#5539,#5540);
#4456=AXIS2_PLACEMENT_3D('',#6658,#5542,#5543);
#4457=AXIS2_PLACEMENT_3D('',#6660,#5544,#5545);
#4458=AXIS2_PLACEMENT_3D('',#6662,#5547,#5548);
#4459=AXIS2_PLACEMENT_3D('',#6664,#5549,#5550);
#4460=AXIS2_PLACEMENT_3D('',#6666,#5552,#5553);
#4461=AXIS2_PLACEMENT_3D('',#6667,#5554,#5555);
#4462=AXIS2_PLACEMENT_3D('',#6676,#5560,#5561);
#4463=AXIS2_PLACEMENT_3D('',#6682,#5565,#5566);
#4464=AXIS2_PLACEMENT_3D('',#6688,#5570,#5571);
#4465=AXIS2_PLACEMENT_3D('',#6694,#5575,#5576);
#4466=AXIS2_PLACEMENT_3D('',#6700,#5580,#5581);
#4467=AXIS2_PLACEMENT_3D('',#6703,#5584,#5585);
#4468=AXIS2_PLACEMENT_3D('',#6704,#5586,#5587);
#4469=AXIS2_PLACEMENT_3D('',#6705,#5588,#5589);
#4470=AXIS2_PLACEMENT_3D('',#6706,#5590,#5591);
#4471=AXIS2_PLACEMENT_3D('',#6708,#5592,#5593);
#4472=AXIS2_PLACEMENT_3D('',#6711,#5595,#5596);
#4473=AXIS2_PLACEMENT_3D('',#6712,#5597,#5598);
#4474=AXIS2_PLACEMENT_3D('',#6714,#5599,#5600);
#4475=AXIS2_PLACEMENT_3D('',#6717,#5602,#5603);
#4476=AXIS2_PLACEMENT_3D('',#6718,#5604,#5605);
#4477=AXIS2_PLACEMENT_3D('',#6719,#5606,#5607);
#4478=AXIS2_PLACEMENT_3D('',#6720,#5608,#5609);
#4479=AXIS2_PLACEMENT_3D('',#6721,#5610,#5611);
#4480=AXIS2_PLACEMENT_3D('',#6733,#5613,#5614);
#4481=AXIS2_PLACEMENT_3D('',#6749,#5615,#5616);
#4482=AXIS2_PLACEMENT_3D('',#6751,#5617,#5618);
#4483=AXIS2_PLACEMENT_3D('',#6777,#5620,#5621);
#4484=AXIS2_PLACEMENT_3D('',#6780,#5624,#5625);
#4485=AXIS2_PLACEMENT_3D('',#6782,#5627,#5628);
#4486=AXIS2_PLACEMENT_3D('',#6784,#5630,#5631);
#4487=AXIS2_PLACEMENT_3D('',#6786,#5632,#5633);
#4488=AXIS2_PLACEMENT_3D('',#6789,#5635,#5636);
#4489=AXIS2_PLACEMENT_3D('',#6790,#5637,#5638);
#4490=AXIS2_PLACEMENT_3D('',#6792,#5640,#5641);
#4491=AXIS2_PLACEMENT_3D('',#6794,#5643,#5644);
#4492=AXIS2_PLACEMENT_3D('',#6795,#5645,#5646);
#4493=AXIS2_PLACEMENT_3D('',#6796,#5647,#5648);
#4494=AXIS2_PLACEMENT_3D('',#6797,#5649,#5650);
#4495=AXIS2_PLACEMENT_3D('',#6798,#5651,#5652);
#4496=AXIS2_PLACEMENT_3D('',#6799,#5653,#5654);
#4497=AXIS2_PLACEMENT_3D('',#6800,#5655,#5656);
#4498=AXIS2_PLACEMENT_3D('',#6801,#5657,#5658);
#4499=AXIS2_PLACEMENT_3D('',#6802,#5659,#5660);
#4500=AXIS2_PLACEMENT_3D('',#6803,#5661,#5662);
#4501=AXIS2_PLACEMENT_3D('',#6804,#5663,#5664);
#4502=AXIS2_PLACEMENT_3D('',#6805,#5665,#5666);
#4503=AXIS2_PLACEMENT_3D('',#6806,#5667,#5668);
#4504=AXIS2_PLACEMENT_3D('',#6807,#5669,#5670);
#4505=AXIS2_PLACEMENT_3D('',#6808,#5671,#5672);
#4506=AXIS2_PLACEMENT_3D('',#6809,#5673,#5674);
#4507=AXIS2_PLACEMENT_3D('',#6810,#5675,#5676);
#4508=AXIS2_PLACEMENT_3D('',#6811,#5677,#5678);
#4509=AXIS2_PLACEMENT_3D('',#6812,#5679,#5680);
#4510=AXIS2_PLACEMENT_3D('',#6813,#5681,#5682);
#4511=AXIS2_PLACEMENT_3D('',#6814,#5683,#5684);
#4512=AXIS2_PLACEMENT_3D('',#6815,#5685,#5686);
#4513=AXIS2_PLACEMENT_3D('',#6816,#5687,#5688);
#4514=AXIS2_PLACEMENT_3D('',#6817,#5689,#5690);
#4515=AXIS2_PLACEMENT_3D('',#6818,#5691,#5692);
#4516=AXIS2_PLACEMENT_3D('',#6819,#5693,#5694);
#4517=AXIS2_PLACEMENT_3D('',#6820,#5695,#5696);
#4518=AXIS2_PLACEMENT_3D('',#6821,#5697,#5698);
#4519=AXIS2_PLACEMENT_3D('',#6822,#5699,#5700);
#4520=AXIS2_PLACEMENT_3D('',#6823,#5701,#5702);
#4521=AXIS2_PLACEMENT_3D('',#6824,#5703,#5704);
#4522=AXIS2_PLACEMENT_3D('',#6825,#5705,#5706);
#4523=AXIS2_PLACEMENT_3D('',#6826,#5707,#5708);
#4524=AXIS2_PLACEMENT_3D('',#6827,#5709,#5710);
#4525=AXIS2_PLACEMENT_3D('',#6828,#5711,#5712);
#4526=AXIS2_PLACEMENT_3D('',#6829,#5713,#5714);
#4527=AXIS2_PLACEMENT_3D('',#6830,#5715,#5716);
#4528=AXIS2_PLACEMENT_3D('',#6831,#5717,#5718);
#4529=AXIS2_PLACEMENT_3D('',#6832,#5719,#5720);
#4530=AXIS2_PLACEMENT_3D('',#6833,#5721,#5722);
#4531=AXIS2_PLACEMENT_3D('',#6834,#5723,#5724);
#4532=AXIS2_PLACEMENT_3D('',#6835,#5725,#5726);
#4533=AXIS2_PLACEMENT_3D('',#6836,#5727,#5728);
#4534=DIRECTION('axis',(0.,0.,1.));
#4535=DIRECTION('refdir',(1.,0.,0.));
#4536=DIRECTION('axis',(0.,0.,1.));
#4537=DIRECTION('refdir',(1.,0.,0.));
#4538=DIRECTION('center_axis',(0.,0.,1.));
#4539=DIRECTION('ref_axis',(1.,0.,0.));
#4540=DIRECTION('center_axis',(0.,0.,1.));
#4541=DIRECTION('ref_axis',(1.,0.,0.));
#4542=DIRECTION('',(0.,0.,1.));
#4543=DIRECTION('center_axis',(0.,0.,-1.));
#4544=DIRECTION('ref_axis',(1.,0.,0.));
#4545=DIRECTION('center_axis',(0.,0.,1.));
#4546=DIRECTION('ref_axis',(1.,0.,0.));
#4547=DIRECTION('center_axis',(0.,0.,1.));
#4548=DIRECTION('ref_axis',(1.,0.,0.));
#4549=DIRECTION('',(0.,0.,1.));
#4550=DIRECTION('center_axis',(0.,0.,-1.));
#4551=DIRECTION('ref_axis',(1.,0.,0.));
#4552=DIRECTION('center_axis',(0.,0.,1.));
#4553=DIRECTION('ref_axis',(1.,0.,0.));
#4554=DIRECTION('center_axis',(0.,0.,1.));
#4555=DIRECTION('ref_axis',(1.,0.,0.));
#4556=DIRECTION('',(0.,0.,1.));
#4557=DIRECTION('center_axis',(0.,0.,-1.));
#4558=DIRECTION('ref_axis',(1.,0.,0.));
#4559=DIRECTION('center_axis',(0.,0.,1.));
#4560=DIRECTION('ref_axis',(1.,0.,0.));
#4561=DIRECTION('center_axis',(0.,0.,1.));
#4562=DIRECTION('ref_axis',(1.,0.,0.));
#4563=DIRECTION('',(0.,0.,1.));
#4564=DIRECTION('center_axis',(0.,0.,-1.));
#4565=DIRECTION('ref_axis',(1.,0.,0.));
#4566=DIRECTION('center_axis',(0.,1.,0.));
#4567=DIRECTION('ref_axis',(-1.,0.,0.));
#4568=DIRECTION('',(-1.,0.,0.));
#4569=DIRECTION('',(0.,0.,1.));
#4570=DIRECTION('',(-1.,0.,0.));
#4571=DIRECTION('',(0.,0.,1.));
#4572=DIRECTION('center_axis',(1.,0.,0.));
#4573=DIRECTION('ref_axis',(0.,1.,0.));
#4574=DIRECTION('',(0.,1.,0.));
#4575=DIRECTION('',(0.,1.,0.));
#4576=DIRECTION('',(0.,0.,1.));
#4577=DIRECTION('center_axis',(0.,-1.,0.));
#4578=DIRECTION('ref_axis',(1.,0.,0.));
#4579=DIRECTION('',(1.,0.,0.));
#4580=DIRECTION('',(1.,0.,0.));
#4581=DIRECTION('',(0.,0.,1.));
#4582=DIRECTION('center_axis',(-1.,0.,0.));
#4583=DIRECTION('ref_axis',(0.,-1.,0.));
#4584=DIRECTION('',(0.,-1.,0.));
#4585=DIRECTION('',(0.,-1.,0.));
#4586=DIRECTION('center_axis',(0.,0.,1.));
#4587=DIRECTION('ref_axis',(1.,0.,0.));
#4588=DIRECTION('center_axis',(0.,0.,1.));
#4589=DIRECTION('ref_axis',(1.,0.,0.));
#4590=DIRECTION('axis',(0.,0.,1.));
#4591=DIRECTION('refdir',(1.,0.,0.));
#4592=DIRECTION('center_axis',(0.,1.,0.));
#4593=DIRECTION('ref_axis',(-1.,0.,0.));
#4594=DIRECTION('',(-1.,0.,0.));
#4595=DIRECTION('',(0.,0.,1.));
#4596=DIRECTION('',(-1.,0.,0.));
#4597=DIRECTION('',(0.,0.,1.));
#4598=DIRECTION('center_axis',(1.,0.,0.));
#4599=DIRECTION('ref_axis',(0.,1.,0.));
#4600=DIRECTION('',(0.,1.,0.));
#4601=DIRECTION('',(0.,1.,0.));
#4602=DIRECTION('',(0.,0.,1.));
#4603=DIRECTION('center_axis',(0.,-1.,0.));
#4604=DIRECTION('ref_axis',(1.,0.,0.));
#4605=DIRECTION('',(1.,0.,0.));
#4606=DIRECTION('',(1.,0.,0.));
#4607=DIRECTION('',(0.,0.,1.));
#4608=DIRECTION('center_axis',(-1.,0.,0.));
#4609=DIRECTION('ref_axis',(0.,-1.,0.));
#4610=DIRECTION('',(0.,-1.,0.));
#4611=DIRECTION('',(0.,-1.,0.));
#4612=DIRECTION('center_axis',(0.,0.,1.));
#4613=DIRECTION('ref_axis',(1.,0.,0.));
#4614=DIRECTION('center_axis',(0.,0.,1.));
#4615=DIRECTION('ref_axis',(1.,0.,0.));
#4616=DIRECTION('axis',(0.,0.,1.));
#4617=DIRECTION('refdir',(1.,0.,0.));
#4618=DIRECTION('center_axis',(0.,1.,0.));
#4619=DIRECTION('ref_axis',(-1.,0.,0.));
#4620=DIRECTION('',(-1.,0.,0.));
#4621=DIRECTION('',(0.,0.,1.));
#4622=DIRECTION('',(-1.,0.,0.));
#4623=DIRECTION('',(0.,0.,1.));
#4624=DIRECTION('center_axis',(1.,0.,0.));
#4625=DIRECTION('ref_axis',(0.,1.,0.));
#4626=DIRECTION('',(0.,1.,0.));
#4627=DIRECTION('',(0.,1.,0.));
#4628=DIRECTION('',(0.,0.,1.));
#4629=DIRECTION('center_axis',(0.,-1.,0.));
#4630=DIRECTION('ref_axis',(1.,0.,0.));
#4631=DIRECTION('',(1.,0.,0.));
#4632=DIRECTION('',(1.,0.,0.));
#4633=DIRECTION('',(0.,0.,1.));
#4634=DIRECTION('center_axis',(-1.,0.,0.));
#4635=DIRECTION('ref_axis',(0.,-1.,0.));
#4636=DIRECTION('',(0.,-1.,0.));
#4637=DIRECTION('',(0.,-1.,0.));
#4638=DIRECTION('center_axis',(0.,0.,1.));
#4639=DIRECTION('ref_axis',(1.,0.,0.));
#4640=DIRECTION('center_axis',(0.,0.,1.));
#4641=DIRECTION('ref_axis',(1.,0.,0.));
#4642=DIRECTION('axis',(0.,0.,1.));
#4643=DIRECTION('refdir',(1.,0.,0.));
#4644=DIRECTION('center_axis',(0.,0.,1.));
#4645=DIRECTION('ref_axis',(1.,0.,0.));
#4646=DIRECTION('center_axis',(0.,0.,1.));
#4647=DIRECTION('ref_axis',(1.,0.,0.));
#4648=DIRECTION('',(0.,0.,1.));
#4649=DIRECTION('center_axis',(0.,0.,-1.));
#4650=DIRECTION('ref_axis',(1.,0.,0.));
#4651=DIRECTION('center_axis',(0.,0.,1.));
#4652=DIRECTION('ref_axis',(1.,0.,0.));
#4653=DIRECTION('center_axis',(0.,0.,1.));
#4654=DIRECTION('ref_axis',(1.,0.,0.));
#4655=DIRECTION('center_axis',(0.,0.,1.));
#4656=DIRECTION('ref_axis',(1.,0.,0.));
#4657=DIRECTION('',(0.,0.,1.));
#4658=DIRECTION('center_axis',(0.,0.,-1.));
#4659=DIRECTION('ref_axis',(1.,0.,0.));
#4660=DIRECTION('center_axis',(0.,0.,1.));
#4661=DIRECTION('ref_axis',(1.,0.,0.));
#4662=DIRECTION('center_axis',(0.,0.,1.));
#4663=DIRECTION('ref_axis',(1.,0.,0.));
#4664=DIRECTION('center_axis',(0.,0.,1.));
#4665=DIRECTION('ref_axis',(1.,0.,0.));
#4666=DIRECTION('',(0.,0.,1.));
#4667=DIRECTION('center_axis',(0.,0.,-1.));
#4668=DIRECTION('ref_axis',(1.,0.,0.));
#4669=DIRECTION('center_axis',(0.,0.,1.));
#4670=DIRECTION('ref_axis',(1.,0.,0.));
#4671=DIRECTION('center_axis',(0.,0.,1.));
#4672=DIRECTION('ref_axis',(1.,0.,0.));
#4673=DIRECTION('',(0.,0.,1.));
#4674=DIRECTION('center_axis',(0.,0.,-1.));
#4675=DIRECTION('ref_axis',(1.,0.,0.));
#4676=DIRECTION('center_axis',(1.,0.,0.));
#4677=DIRECTION('ref_axis',(0.,0.,-1.));
#4678=DIRECTION('',(-1.,0.,0.));
#4679=DIRECTION('center_axis',(-1.,0.,0.));
#4680=DIRECTION('ref_axis',(0.,0.,-1.));
#4681=DIRECTION('',(1.,0.,0.));
#4682=DIRECTION('center_axis',(1.,0.,0.));
#4683=DIRECTION('ref_axis',(0.,0.,-1.));
#4684=DIRECTION('center_axis',(1.,0.,0.));
#4685=DIRECTION('ref_axis',(0.,0.,-1.));
#4686=DIRECTION('',(0.,-1.,0.));
#4687=DIRECTION('',(0.,0.,-1.));
#4688=DIRECTION('',(0.,1.,0.));
#4689=DIRECTION('',(0.,0.,-1.));
#4690=DIRECTION('',(0.,-1.,0.));
#4691=DIRECTION('',(0.,0.,-1.));
#4692=DIRECTION('',(0.,1.,0.));
#4693=DIRECTION('',(0.,0.,1.));
#4694=DIRECTION('',(0.,-1.,0.));
#4695=DIRECTION('',(0.,0.,1.));
#4696=DIRECTION('',(0.,1.,0.));
#4697=DIRECTION('',(0.,0.,1.));
#4698=DIRECTION('',(0.,-1.,0.));
#4699=DIRECTION('center_axis',(0.,0.,1.));
#4700=DIRECTION('ref_axis',(0.,-1.,0.));
#4701=DIRECTION('',(0.,-1.,0.));
#4702=DIRECTION('',(1.,0.,0.));
#4703=DIRECTION('center_axis',(0.,0.,1.));
#4704=DIRECTION('ref_axis',(0.,-1.,0.));
#4705=DIRECTION('',(1.,0.,0.));
#4706=DIRECTION('',(0.,-1.,0.));
#4707=DIRECTION('center_axis',(0.,0.,1.));
#4708=DIRECTION('ref_axis',(0.,-1.,0.));
#4709=DIRECTION('',(0.,-1.,0.));
#4710=DIRECTION('',(1.,0.,0.));
#4711=DIRECTION('',(1.,0.,0.));
#4712=DIRECTION('center_axis',(0.,-1.,0.));
#4713=DIRECTION('ref_axis',(0.,0.,-1.));
#4714=DIRECTION('',(0.,0.,-1.));
#4715=DIRECTION('',(1.,0.,0.));
#4716=DIRECTION('center_axis',(0.,0.,-1.));
#4717=DIRECTION('ref_axis',(0.,1.,0.));
#4718=DIRECTION('',(0.,1.,0.));
#4719=DIRECTION('',(1.,0.,0.));
#4720=DIRECTION('center_axis',(0.,-1.,0.));
#4721=DIRECTION('ref_axis',(0.,0.,-1.));
#4722=DIRECTION('',(0.,0.,-1.));
#4723=DIRECTION('center_axis',(0.,1.,0.));
#4724=DIRECTION('ref_axis',(0.,0.,1.));
#4725=DIRECTION('',(0.,0.,1.));
#4726=DIRECTION('',(1.,0.,0.));
#4727=DIRECTION('center_axis',(0.,0.,-1.));
#4728=DIRECTION('ref_axis',(0.,1.,0.));
#4729=DIRECTION('',(0.,1.,0.));
#4730=DIRECTION('',(1.,0.,0.));
#4731=DIRECTION('center_axis',(0.,1.,0.));
#4732=DIRECTION('ref_axis',(0.,0.,1.));
#4733=DIRECTION('',(0.,0.,1.));
#4734=DIRECTION('',(1.,0.,0.));
#4735=DIRECTION('center_axis',(0.,0.,1.));
#4736=DIRECTION('ref_axis',(0.,-1.,0.));
#4737=DIRECTION('',(0.,-1.,0.));
#4738=DIRECTION('',(1.,0.,0.));
#4739=DIRECTION('center_axis',(0.,1.,0.));
#4740=DIRECTION('ref_axis',(0.,0.,1.));
#4741=DIRECTION('',(0.,0.,1.));
#4742=DIRECTION('',(1.,0.,0.));
#4743=DIRECTION('center_axis',(0.,0.,-1.));
#4744=DIRECTION('ref_axis',(0.,1.,0.));
#4745=DIRECTION('',(0.,1.,0.));
#4746=DIRECTION('',(1.,0.,0.));
#4747=DIRECTION('center_axis',(0.,-1.,0.));
#4748=DIRECTION('ref_axis',(0.,0.,-1.));
#4749=DIRECTION('',(0.,0.,-1.));
#4750=DIRECTION('center_axis',(1.,0.,0.));
#4751=DIRECTION('ref_axis',(0.,0.,-1.));
#4752=DIRECTION('axis',(0.,0.,1.));
#4753=DIRECTION('refdir',(1.,0.,0.));
#4754=DIRECTION('center_axis',(0.,0.,1.));
#4755=DIRECTION('ref_axis',(1.,0.,0.));
#4756=DIRECTION('',(-1.,0.,0.));
#4757=DIRECTION('center_axis',(0.,0.,1.));
#4758=DIRECTION('ref_axis',(1.,0.,0.));
#4759=DIRECTION('center_axis',(0.,0.,1.));
#4760=DIRECTION('ref_axis',(1.,0.,0.));
#4761=DIRECTION('center_axis',(0.,0.,1.));
#4762=DIRECTION('ref_axis',(6.12323399573677E-17,1.,0.));
#4763=DIRECTION('',(0.,0.,-1.));
#4764=DIRECTION('center_axis',(0.,0.,-1.));
#4765=DIRECTION('ref_axis',(1.,0.,0.));
#4766=DIRECTION('',(0.,0.,1.));
#4767=DIRECTION('center_axis',(0.,0.,1.));
#4768=DIRECTION('ref_axis',(1.,0.,0.));
#4769=DIRECTION('',(1.,0.,0.));
#4770=DIRECTION('center_axis',(0.,0.,1.));
#4771=DIRECTION('ref_axis',(1.,0.,0.));
#4772=DIRECTION('center_axis',(0.,0.,1.));
#4773=DIRECTION('ref_axis',(1.,0.,0.));
#4774=DIRECTION('center_axis',(0.,0.,1.));
#4775=DIRECTION('ref_axis',(-1.83697019872103E-16,-1.,0.));
#4776=DIRECTION('',(0.,0.,-1.));
#4777=DIRECTION('center_axis',(0.,0.,-1.));
#4778=DIRECTION('ref_axis',(1.,0.,0.));
#4779=DIRECTION('',(0.,0.,1.));
#4780=DIRECTION('center_axis',(0.,-1.,0.));
#4781=DIRECTION('ref_axis',(1.,0.,0.));
#4782=DIRECTION('',(1.,0.,0.));
#4783=DIRECTION('',(0.,0.,1.));
#4784=DIRECTION('',(1.,0.,0.));
#4785=DIRECTION('',(0.,0.,1.));
#4786=DIRECTION('',(1.,0.,0.));
#4787=DIRECTION('center_axis',(0.,1.,0.));
#4788=DIRECTION('ref_axis',(-1.,0.,0.));
#4789=DIRECTION('',(-1.,0.,0.));
#4790=DIRECTION('',(0.,0.,1.));
#4791=DIRECTION('',(-1.,0.,0.));
#4792=DIRECTION('',(0.,0.,1.));
#4793=DIRECTION('',(-1.,0.,0.));
#4794=DIRECTION('center_axis',(0.,0.,1.));
#4795=DIRECTION('ref_axis',(1.,0.,0.));
#4796=DIRECTION('center_axis',(0.,0.,1.));
#4797=DIRECTION('ref_axis',(1.,0.,0.));
#4798=DIRECTION('',(0.,0.,1.));
#4799=DIRECTION('center_axis',(0.,0.,1.));
#4800=DIRECTION('ref_axis',(1.,0.,0.));
#4801=DIRECTION('center_axis',(0.,0.,1.));
#4802=DIRECTION('ref_axis',(1.,0.,0.));
#4803=DIRECTION('',(0.,0.,1.));
#4804=DIRECTION('center_axis',(1.,0.,0.));
#4805=DIRECTION('ref_axis',(0.,1.22464679914735E-16,1.));
#4806=DIRECTION('center_axis',(1.,0.,0.));
#4807=DIRECTION('ref_axis',(0.,0.,-1.));
#4808=DIRECTION('',(-1.,0.,0.));
#4809=DIRECTION('center_axis',(-1.,0.,0.));
#4810=DIRECTION('ref_axis',(0.,0.,-1.));
#4811=DIRECTION('',(1.,0.,0.));
#4812=DIRECTION('center_axis',(1.,0.,0.));
#4813=DIRECTION('ref_axis',(0.,1.,0.));
#4814=DIRECTION('',(0.,1.,0.));
#4815=DIRECTION('',(0.,1.,0.));
#4816=DIRECTION('',(0.,1.,0.));
#4817=DIRECTION('center_axis',(0.,0.,1.));
#4818=DIRECTION('ref_axis',(1.,0.,0.));
#4819=DIRECTION('',(0.,-1.,0.));
#4820=DIRECTION('center_axis',(-1.,0.,0.));
#4821=DIRECTION('ref_axis',(0.,-1.,0.));
#4822=DIRECTION('',(0.,-1.,0.));
#4823=DIRECTION('',(0.,-1.,0.));
#4824=DIRECTION('center_axis',(0.,0.,1.));
#4825=DIRECTION('ref_axis',(1.,0.,0.));
#4826=DIRECTION('center_axis',(0.,0.,1.));
#4827=DIRECTION('ref_axis',(1.,0.,0.));
#4828=DIRECTION('axis',(0.,0.,1.));
#4829=DIRECTION('refdir',(1.,0.,0.));
#4830=DIRECTION('center_axis',(0.,0.,1.));
#4831=DIRECTION('ref_axis',(1.,0.,0.));
#4832=DIRECTION('center_axis',(0.,0.,1.));
#4833=DIRECTION('ref_axis',(1.,0.,0.));
#4834=DIRECTION('',(0.,0.,1.));
#4835=DIRECTION('center_axis',(0.,0.,-1.));
#4836=DIRECTION('ref_axis',(1.,0.,0.));
#4837=DIRECTION('center_axis',(0.,0.,1.));
#4838=DIRECTION('ref_axis',(1.,0.,0.));
#4839=DIRECTION('center_axis',(0.,0.,1.));
#4840=DIRECTION('ref_axis',(1.,0.,0.));
#4841=DIRECTION('center_axis',(0.,0.,1.));
#4842=DIRECTION('ref_axis',(1.,0.,0.));
#4843=DIRECTION('',(0.,0.,1.));
#4844=DIRECTION('center_axis',(0.,0.,-1.));
#4845=DIRECTION('ref_axis',(1.,0.,0.));
#4846=DIRECTION('center_axis',(0.,0.,1.));
#4847=DIRECTION('ref_axis',(1.,0.,0.));
#4848=DIRECTION('center_axis',(0.,0.,1.));
#4849=DIRECTION('ref_axis',(1.,0.,0.));
#4850=DIRECTION('center_axis',(0.,0.,1.));
#4851=DIRECTION('ref_axis',(1.,0.,0.));
#4852=DIRECTION('',(0.,0.,1.));
#4853=DIRECTION('center_axis',(0.,0.,-1.));
#4854=DIRECTION('ref_axis',(1.,0.,0.));
#4855=DIRECTION('center_axis',(0.,0.,1.));
#4856=DIRECTION('ref_axis',(1.,0.,0.));
#4857=DIRECTION('center_axis',(0.,0.,1.));
#4858=DIRECTION('ref_axis',(1.,0.,0.));
#4859=DIRECTION('',(0.,0.,1.));
#4860=DIRECTION('center_axis',(0.,0.,-1.));
#4861=DIRECTION('ref_axis',(1.,0.,0.));
#4862=DIRECTION('center_axis',(1.,0.,0.));
#4863=DIRECTION('ref_axis',(0.,0.,-1.));
#4864=DIRECTION('',(-1.,0.,0.));
#4865=DIRECTION('center_axis',(-1.,0.,0.));
#4866=DIRECTION('ref_axis',(0.,0.,-1.));
#4867=DIRECTION('',(1.,0.,0.));
#4868=DIRECTION('center_axis',(1.,0.,0.));
#4869=DIRECTION('ref_axis',(0.,0.,-1.));
#4870=DIRECTION('center_axis',(1.,0.,0.));
#4871=DIRECTION('ref_axis',(0.,0.,-1.));
#4872=DIRECTION('',(0.,-1.,0.));
#4873=DIRECTION('',(0.,0.,-1.));
#4874=DIRECTION('',(0.,1.,0.));
#4875=DIRECTION('',(0.,0.,-1.));
#4876=DIRECTION('',(0.,-1.,0.));
#4877=DIRECTION('',(0.,0.,-1.));
#4878=DIRECTION('',(0.,1.,0.));
#4879=DIRECTION('',(0.,0.,1.));
#4880=DIRECTION('',(0.,-1.,0.));
#4881=DIRECTION('',(0.,0.,1.));
#4882=DIRECTION('',(0.,1.,0.));
#4883=DIRECTION('',(0.,0.,1.));
#4884=DIRECTION('',(0.,-1.,0.));
#4885=DIRECTION('center_axis',(0.,0.,1.));
#4886=DIRECTION('ref_axis',(0.,-1.,0.));
#4887=DIRECTION('',(0.,-1.,0.));
#4888=DIRECTION('',(1.,0.,0.));
#4889=DIRECTION('center_axis',(0.,0.,1.));
#4890=DIRECTION('ref_axis',(0.,-1.,0.));
#4891=DIRECTION('',(1.,0.,0.));
#4892=DIRECTION('',(0.,-1.,0.));
#4893=DIRECTION('center_axis',(0.,0.,1.));
#4894=DIRECTION('ref_axis',(0.,-1.,0.));
#4895=DIRECTION('',(0.,-1.,0.));
#4896=DIRECTION('',(1.,0.,0.));
#4897=DIRECTION('',(1.,0.,0.));
#4898=DIRECTION('center_axis',(0.,-1.,0.));
#4899=DIRECTION('ref_axis',(0.,0.,-1.));
#4900=DIRECTION('',(0.,0.,-1.));
#4901=DIRECTION('',(1.,0.,0.));
#4902=DIRECTION('center_axis',(0.,0.,-1.));
#4903=DIRECTION('ref_axis',(0.,1.,0.));
#4904=DIRECTION('',(0.,1.,0.));
#4905=DIRECTION('',(1.,0.,0.));
#4906=DIRECTION('center_axis',(0.,-1.,0.));
#4907=DIRECTION('ref_axis',(0.,0.,-1.));
#4908=DIRECTION('',(0.,0.,-1.));
#4909=DIRECTION('center_axis',(0.,1.,0.));
#4910=DIRECTION('ref_axis',(0.,0.,1.));
#4911=DIRECTION('',(0.,0.,1.));
#4912=DIRECTION('',(1.,0.,0.));
#4913=DIRECTION('center_axis',(0.,0.,-1.));
#4914=DIRECTION('ref_axis',(0.,1.,0.));
#4915=DIRECTION('',(0.,1.,0.));
#4916=DIRECTION('',(1.,0.,0.));
#4917=DIRECTION('center_axis',(0.,1.,0.));
#4918=DIRECTION('ref_axis',(0.,0.,1.));
#4919=DIRECTION('',(0.,0.,1.));
#4920=DIRECTION('',(1.,0.,0.));
#4921=DIRECTION('center_axis',(0.,0.,1.));
#4922=DIRECTION('ref_axis',(0.,-1.,0.));
#4923=DIRECTION('',(0.,-1.,0.));
#4924=DIRECTION('',(1.,0.,0.));
#4925=DIRECTION('center_axis',(0.,1.,0.));
#4926=DIRECTION('ref_axis',(0.,0.,1.));
#4927=DIRECTION('',(0.,0.,1.));
#4928=DIRECTION('',(1.,0.,0.));
#4929=DIRECTION('center_axis',(0.,0.,-1.));
#4930=DIRECTION('ref_axis',(0.,1.,0.));
#4931=DIRECTION('',(0.,1.,0.));
#4932=DIRECTION('',(1.,0.,0.));
#4933=DIRECTION('center_axis',(0.,-1.,0.));
#4934=DIRECTION('ref_axis',(0.,0.,-1.));
#4935=DIRECTION('',(0.,0.,-1.));
#4936=DIRECTION('center_axis',(1.,0.,0.));
#4937=DIRECTION('ref_axis',(0.,0.,-1.));
#4938=DIRECTION('axis',(0.,0.,1.));
#4939=DIRECTION('refdir',(1.,0.,0.));
#4940=DIRECTION('center_axis',(0.,0.,1.));
#4941=DIRECTION('ref_axis',(1.,0.,0.));
#4942=DIRECTION('',(-1.,0.,0.));
#4943=DIRECTION('center_axis',(0.,0.,1.));
#4944=DIRECTION('ref_axis',(1.,0.,0.));
#4945=DIRECTION('center_axis',(0.,0.,1.));
#4946=DIRECTION('ref_axis',(1.,0.,0.));
#4947=DIRECTION('center_axis',(0.,0.,1.));
#4948=DIRECTION('ref_axis',(6.12323399573677E-17,1.,0.));
#4949=DIRECTION('',(0.,0.,-1.));
#4950=DIRECTION('center_axis',(0.,0.,-1.));
#4951=DIRECTION('ref_axis',(1.,0.,0.));
#4952=DIRECTION('',(0.,0.,1.));
#4953=DIRECTION('center_axis',(0.,0.,1.));
#4954=DIRECTION('ref_axis',(1.,0.,0.));
#4955=DIRECTION('',(1.,0.,0.));
#4956=DIRECTION('center_axis',(0.,0.,1.));
#4957=DIRECTION('ref_axis',(1.,0.,0.));
#4958=DIRECTION('center_axis',(0.,0.,1.));
#4959=DIRECTION('ref_axis',(1.,0.,0.));
#4960=DIRECTION('center_axis',(0.,0.,1.));
#4961=DIRECTION('ref_axis',(-1.83697019872103E-16,-1.,0.));
#4962=DIRECTION('',(0.,0.,-1.));
#4963=DIRECTION('center_axis',(0.,0.,-1.));
#4964=DIRECTION('ref_axis',(1.,0.,0.));
#4965=DIRECTION('',(0.,0.,1.));
#4966=DIRECTION('center_axis',(0.,-1.,0.));
#4967=DIRECTION('ref_axis',(1.,0.,0.));
#4968=DIRECTION('',(1.,0.,0.));
#4969=DIRECTION('',(0.,0.,1.));
#4970=DIRECTION('',(1.,0.,0.));
#4971=DIRECTION('',(0.,0.,1.));
#4972=DIRECTION('',(1.,0.,0.));
#4973=DIRECTION('center_axis',(0.,1.,0.));
#4974=DIRECTION('ref_axis',(-1.,0.,0.));
#4975=DIRECTION('',(-1.,0.,0.));
#4976=DIRECTION('',(0.,0.,1.));
#4977=DIRECTION('',(-1.,0.,0.));
#4978=DIRECTION('',(0.,0.,1.));
#4979=DIRECTION('',(-1.,0.,0.));
#4980=DIRECTION('center_axis',(0.,0.,1.));
#4981=DIRECTION('ref_axis',(1.,0.,0.));
#4982=DIRECTION('center_axis',(0.,0.,1.));
#4983=DIRECTION('ref_axis',(1.,0.,0.));
#4984=DIRECTION('',(0.,0.,1.));
#4985=DIRECTION('center_axis',(0.,0.,1.));
#4986=DIRECTION('ref_axis',(1.,0.,0.));
#4987=DIRECTION('center_axis',(0.,0.,1.));
#4988=DIRECTION('ref_axis',(1.,0.,0.));
#4989=DIRECTION('',(0.,0.,1.));
#4990=DIRECTION('center_axis',(1.,0.,0.));
#4991=DIRECTION('ref_axis',(0.,1.22464679914735E-16,1.));
#4992=DIRECTION('center_axis',(1.,0.,0.));
#4993=DIRECTION('ref_axis',(0.,0.,-1.));
#4994=DIRECTION('',(-1.,0.,0.));
#4995=DIRECTION('center_axis',(-1.,0.,0.));
#4996=DIRECTION('ref_axis',(0.,0.,-1.));
#4997=DIRECTION('',(1.,0.,0.));
#4998=DIRECTION('center_axis',(1.,0.,0.));
#4999=DIRECTION('ref_axis',(0.,1.,0.));
#5000=DIRECTION('',(0.,1.,0.));
#5001=DIRECTION('',(0.,1.,0.));
#5002=DIRECTION('',(0.,1.,0.));
#5003=DIRECTION('center_axis',(0.,0.,1.));
#5004=DIRECTION('ref_axis',(1.,0.,0.));
#5005=DIRECTION('',(0.,-1.,0.));
#5006=DIRECTION('center_axis',(-1.,0.,0.));
#5007=DIRECTION('ref_axis',(0.,-1.,0.));
#5008=DIRECTION('',(0.,-1.,0.));
#5009=DIRECTION('',(0.,-1.,0.));
#5010=DIRECTION('center_axis',(0.,0.,1.));
#5011=DIRECTION('ref_axis',(1.,0.,0.));
#5012=DIRECTION('center_axis',(0.,0.,1.));
#5013=DIRECTION('ref_axis',(1.,0.,0.));
#5014=DIRECTION('axis',(0.,0.,1.));
#5015=DIRECTION('refdir',(1.,0.,0.));
#5016=DIRECTION('center_axis',(1.,0.,0.));
#5017=DIRECTION('ref_axis',(0.,0.,-1.));
#5018=DIRECTION('center_axis',(1.,0.,0.));
#5019=DIRECTION('ref_axis',(0.,0.,-1.));
#5020=DIRECTION('',(1.,0.,0.));
#5021=DIRECTION('center_axis',(1.,0.,0.));
#5022=DIRECTION('ref_axis',(0.,0.,-1.));
#5023=DIRECTION('center_axis',(1.,0.,0.));
#5024=DIRECTION('ref_axis',(0.,0.,-1.));
#5025=DIRECTION('center_axis',(-1.,0.,0.));
#5026=DIRECTION('ref_axis',(0.,0.,-1.));
#5027=DIRECTION('center_axis',(1.,0.,0.));
#5028=DIRECTION('ref_axis',(0.,0.,-1.));
#5029=DIRECTION('center_axis',(-1.,0.,0.));
#5030=DIRECTION('ref_axis',(0.,0.,-1.));
#5031=DIRECTION('',(-1.,0.,0.));
#5032=DIRECTION('center_axis',(1.,0.,0.));
#5033=DIRECTION('ref_axis',(0.,0.,-1.));
#5034=DIRECTION('center_axis',(1.,0.,0.));
#5035=DIRECTION('ref_axis',(0.,0.,-1.));
#5036=DIRECTION('',(-1.,0.,0.));
#5037=DIRECTION('center_axis',(1.,0.,0.));
#5038=DIRECTION('ref_axis',(0.,0.,-1.));
#5039=DIRECTION('center_axis',(1.,0.,0.));
#5040=DIRECTION('ref_axis',(0.,0.,-1.));
#5041=DIRECTION('center_axis',(1.,0.,0.));
#5042=DIRECTION('ref_axis',(0.,0.,-1.));
#5043=DIRECTION('axis',(0.,0.,1.));
#5044=DIRECTION('refdir',(1.,0.,0.));
#5045=DIRECTION('center_axis',(1.,0.,0.));
#5046=DIRECTION('ref_axis',(0.,0.,-1.));
#5047=DIRECTION('center_axis',(1.,0.,0.));
#5048=DIRECTION('ref_axis',(0.,0.,-1.));
#5049=DIRECTION('',(1.,0.,0.));
#5050=DIRECTION('center_axis',(-1.,0.,0.));
#5051=DIRECTION('ref_axis',(0.,0.,-1.));
#5052=DIRECTION('center_axis',(1.,0.,0.));
#5053=DIRECTION('ref_axis',(0.,0.,-1.));
#5054=DIRECTION('center_axis',(1.,0.,0.));
#5055=DIRECTION('ref_axis',(0.,0.,-1.));
#5056=DIRECTION('',(1.,0.,0.));
#5057=DIRECTION('center_axis',(-1.,0.,0.));
#5058=DIRECTION('ref_axis',(0.,0.,-1.));
#5059=DIRECTION('center_axis',(1.,0.,0.));
#5060=DIRECTION('ref_axis',(0.,0.,-1.));
#5061=DIRECTION('center_axis',(1.,0.,0.));
#5062=DIRECTION('ref_axis',(0.,0.,-1.));
#5063=DIRECTION('',(1.,0.,0.));
#5064=DIRECTION('center_axis',(-1.,0.,0.));
#5065=DIRECTION('ref_axis',(0.,0.,-1.));
#5066=DIRECTION('center_axis',(1.,0.,0.));
#5067=DIRECTION('ref_axis',(0.,0.,-1.));
#5068=DIRECTION('center_axis',(1.,0.,0.));
#5069=DIRECTION('ref_axis',(0.,0.,-1.));
#5070=DIRECTION('',(1.,0.,0.));
#5071=DIRECTION('center_axis',(-1.,0.,0.));
#5072=DIRECTION('ref_axis',(0.,0.,-1.));
#5073=DIRECTION('center_axis',(1.,0.,0.));
#5074=DIRECTION('ref_axis',(0.,0.,-1.));
#5075=DIRECTION('center_axis',(1.,0.,0.));
#5076=DIRECTION('ref_axis',(0.,0.,-1.));
#5077=DIRECTION('center_axis',(-1.,0.,0.));
#5078=DIRECTION('ref_axis',(0.,0.,-1.));
#5079=DIRECTION('center_axis',(1.,0.,0.));
#5080=DIRECTION('ref_axis',(0.,0.,-1.));
#5081=DIRECTION('center_axis',(1.,0.,0.));
#5082=DIRECTION('ref_axis',(0.,0.,-1.));
#5083=DIRECTION('',(-1.,0.,0.));
#5084=DIRECTION('center_axis',(1.,0.,0.));
#5085=DIRECTION('ref_axis',(0.,0.,-1.));
#5086=DIRECTION('center_axis',(-1.,0.,0.));
#5087=DIRECTION('ref_axis',(0.,0.,-1.));
#5088=DIRECTION('',(-1.,0.,0.));
#5089=DIRECTION('center_axis',(-1.,0.,0.));
#5090=DIRECTION('ref_axis',(0.,0.,-1.));
#5091=DIRECTION('center_axis',(1.,0.,0.));
#5092=DIRECTION('ref_axis',(0.,0.,-1.));
#5093=DIRECTION('',(-1.,0.,0.));
#5094=DIRECTION('center_axis',(1.,0.,0.));
#5095=DIRECTION('ref_axis',(0.,0.,-1.));
#5096=DIRECTION('center_axis',(1.,0.,0.));
#5097=DIRECTION('ref_axis',(0.,0.,-1.));
#5098=DIRECTION('center_axis',(1.,0.,0.));
#5099=DIRECTION('ref_axis',(0.,0.,-1.));
#5100=DIRECTION('axis',(0.,0.,1.));
#5101=DIRECTION('refdir',(1.,0.,0.));
#5102=DIRECTION('center_axis',(1.,0.,0.));
#5103=DIRECTION('ref_axis',(0.,0.,-1.));
#5104=DIRECTION('center_axis',(1.,0.,0.));
#5105=DIRECTION('ref_axis',(0.,0.,-1.));
#5106=DIRECTION('',(1.,0.,0.));
#5107=DIRECTION('center_axis',(-1.,0.,0.));
#5108=DIRECTION('ref_axis',(0.,0.,-1.));
#5109=DIRECTION('center_axis',(1.,0.,0.));
#5110=DIRECTION('ref_axis',(0.,0.,-1.));
#5111=DIRECTION('center_axis',(1.,0.,0.));
#5112=DIRECTION('ref_axis',(0.,0.,-1.));
#5113=DIRECTION('center_axis',(1.,0.,0.));
#5114=DIRECTION('ref_axis',(0.,0.,-1.));
#5115=DIRECTION('',(-1.,0.,0.));
#5116=DIRECTION('center_axis',(-1.,0.,0.));
#5117=DIRECTION('ref_axis',(0.,0.,-1.));
#5118=DIRECTION('center_axis',(1.,0.,0.));
#5119=DIRECTION('ref_axis',(0.,0.,-1.));
#5120=DIRECTION('center_axis',(1.,0.,0.));
#5121=DIRECTION('ref_axis',(0.,0.,-1.));
#5122=DIRECTION('',(-1.,0.,0.));
#5123=DIRECTION('center_axis',(1.,0.,0.));
#5124=DIRECTION('ref_axis',(0.,0.,-1.));
#5125=DIRECTION('center_axis',(1.,0.,0.));
#5126=DIRECTION('ref_axis',(0.,0.,-1.));
#5127=DIRECTION('center_axis',(1.,0.,0.));
#5128=DIRECTION('ref_axis',(0.,0.,-1.));
#5129=DIRECTION('axis',(0.,0.,1.));
#5130=DIRECTION('refdir',(1.,0.,0.));
#5131=DIRECTION('center_axis',(1.,0.,0.));
#5132=DIRECTION('ref_axis',(0.,0.,-1.));
#5133=DIRECTION('center_axis',(1.,0.,0.));
#5134=DIRECTION('ref_axis',(0.,0.,-1.));
#5135=DIRECTION('',(1.,0.,0.));
#5136=DIRECTION('center_axis',(-1.,0.,0.));
#5137=DIRECTION('ref_axis',(0.,0.,-1.));
#5138=DIRECTION('center_axis',(1.,0.,0.));
#5139=DIRECTION('ref_axis',(0.,0.,-1.));
#5140=DIRECTION('center_axis',(1.,0.,0.));
#5141=DIRECTION('ref_axis',(0.,0.,-1.));
#5142=DIRECTION('',(1.,0.,0.));
#5143=DIRECTION('center_axis',(-1.,0.,0.));
#5144=DIRECTION('ref_axis',(0.,0.,-1.));
#5145=DIRECTION('center_axis',(1.,0.,0.));
#5146=DIRECTION('ref_axis',(0.,0.,-1.));
#5147=DIRECTION('center_axis',(1.,0.,0.));
#5148=DIRECTION('ref_axis',(0.,0.,-1.));
#5149=DIRECTION('',(1.,0.,0.));
#5150=DIRECTION('center_axis',(-1.,0.,0.));
#5151=DIRECTION('ref_axis',(0.,0.,-1.));
#5152=DIRECTION('center_axis',(1.,0.,0.));
#5153=DIRECTION('ref_axis',(0.,0.,-1.));
#5154=DIRECTION('center_axis',(1.,0.,0.));
#5155=DIRECTION('ref_axis',(0.,0.,-1.));
#5156=DIRECTION('',(1.,0.,0.));
#5157=DIRECTION('center_axis',(-1.,0.,0.));
#5158=DIRECTION('ref_axis',(0.,0.,-1.));
#5159=DIRECTION('center_axis',(1.,0.,0.));
#5160=DIRECTION('ref_axis',(0.,0.,-1.));
#5161=DIRECTION('center_axis',(1.,0.,0.));
#5162=DIRECTION('ref_axis',(0.,0.,-1.));
#5163=DIRECTION('center_axis',(1.,0.,0.));
#5164=DIRECTION('ref_axis',(0.,0.,-1.));
#5165=DIRECTION('center_axis',(1.,0.,0.));
#5166=DIRECTION('ref_axis',(0.,0.,-1.));
#5167=DIRECTION('',(-1.,0.,0.));
#5168=DIRECTION('center_axis',(1.,0.,0.));
#5169=DIRECTION('ref_axis',(0.,0.,-1.));
#5170=DIRECTION('center_axis',(1.,0.,0.));
#5171=DIRECTION('ref_axis',(0.,0.,-1.));
#5172=DIRECTION('center_axis',(-1.,0.,0.));
#5173=DIRECTION('ref_axis',(0.,0.,-1.));
#5174=DIRECTION('',(-1.,0.,0.));
#5175=DIRECTION('center_axis',(-1.,0.,0.));
#5176=DIRECTION('ref_axis',(0.,0.,-1.));
#5177=DIRECTION('center_axis',(1.,0.,0.));
#5178=DIRECTION('ref_axis',(0.,0.,-1.));
#5179=DIRECTION('center_axis',(1.,0.,0.));
#5180=DIRECTION('ref_axis',(0.,0.,-1.));
#5181=DIRECTION('',(-1.,0.,0.));
#5182=DIRECTION('center_axis',(1.,0.,0.));
#5183=DIRECTION('ref_axis',(0.,0.,-1.));
#5184=DIRECTION('center_axis',(1.,0.,0.));
#5185=DIRECTION('ref_axis',(0.,0.,-1.));
#5186=DIRECTION('axis',(0.,0.,1.));
#5187=DIRECTION('refdir',(1.,0.,0.));
#5188=DIRECTION('center_axis',(1.,0.,0.));
#5189=DIRECTION('ref_axis',(0.,0.,-1.));
#5190=DIRECTION('center_axis',(-1.,0.,0.));
#5191=DIRECTION('ref_axis',(0.,0.,-1.));
#5192=DIRECTION('',(-1.,0.,0.));
#5193=DIRECTION('center_axis',(-1.,0.,0.));
#5194=DIRECTION('ref_axis',(0.,0.,-1.));
#5195=DIRECTION('center_axis',(1.,0.,0.));
#5196=DIRECTION('ref_axis',(0.,0.,-1.));
#5197=DIRECTION('center_axis',(1.,0.,0.));
#5198=DIRECTION('ref_axis',(0.,0.,-1.));
#5199=DIRECTION('',(-1.,0.,0.));
#5200=DIRECTION('center_axis',(1.,0.,0.));
#5201=DIRECTION('ref_axis',(0.,0.,-1.));
#5202=DIRECTION('center_axis',(1.,0.,0.));
#5203=DIRECTION('ref_axis',(0.,0.,-1.));
#5204=DIRECTION('center_axis',(1.,0.,0.));
#5205=DIRECTION('ref_axis',(0.,0.,-1.));
#5206=DIRECTION('axis',(0.,0.,1.));
#5207=DIRECTION('refdir',(1.,0.,0.));
#5208=DIRECTION('center_axis',(0.866025403784439,0.,-0.5));
#5209=DIRECTION('ref_axis',(0.5,0.,0.866025403784439));
#5210=DIRECTION('',(-0.5,0.,-0.866025403784439));
#5211=DIRECTION('',(0.,-1.,0.));
#5212=DIRECTION('',(0.5,0.,0.866025403784439));
#5213=DIRECTION('',(0.,-1.,0.));
#5214=DIRECTION('center_axis',(1.20185167898973E-16,0.,-1.));
#5215=DIRECTION('ref_axis',(1.,0.,1.20185167898973E-16));
#5216=DIRECTION('',(-1.,0.,-1.20185167898973E-16));
#5217=DIRECTION('',(0.,-1.,0.));
#5218=DIRECTION('',(1.,0.,1.20185167898973E-16));
#5219=DIRECTION('center_axis',(-0.866025403784439,0.,-0.5));
#5220=DIRECTION('ref_axis',(0.5,0.,-0.866025403784439));
#5221=DIRECTION('',(-0.5,0.,0.866025403784439));
#5222=DIRECTION('',(0.,-1.,0.));
#5223=DIRECTION('',(0.5,0.,-0.866025403784439));
#5224=DIRECTION('center_axis',(-0.866025403784439,0.,0.5));
#5225=DIRECTION('ref_axis',(-0.5,0.,-0.866025403784439));
#5226=DIRECTION('',(0.5,0.,0.866025403784439));
#5227=DIRECTION('',(0.,-1.,0.));
#5228=DIRECTION('',(-0.5,0.,-0.866025403784439));
#5229=DIRECTION('center_axis',(-2.40370335797945E-16,0.,1.));
#5230=DIRECTION('ref_axis',(-1.,0.,-2.40370335797945E-16));
#5231=DIRECTION('',(1.,0.,2.40370335797945E-16));
#5232=DIRECTION('',(0.,-1.,0.));
#5233=DIRECTION('',(-1.,0.,-2.40370335797945E-16));
#5234=DIRECTION('center_axis',(0.866025403784439,0.,0.5));
#5235=DIRECTION('ref_axis',(-0.5,0.,0.866025403784439));
#5236=DIRECTION('',(0.5,0.,-0.866025403784439));
#5237=DIRECTION('',(-0.5,0.,0.866025403784439));
#5238=DIRECTION('center_axis',(0.,1.,0.));
#5239=DIRECTION('ref_axis',(1.,0.,0.));
#5240=DIRECTION('center_axis',(0.,-1.,0.));
#5241=DIRECTION('ref_axis',(0.,0.,-1.));
#5242=DIRECTION('center_axis',(0.,1.,0.));
#5243=DIRECTION('ref_axis',(1.,0.,0.));
#5244=DIRECTION('center_axis',(0.,1.,0.));
#5245=DIRECTION('ref_axis',(1.,0.,0.));
#5246=DIRECTION('center_axis',(0.,1.,0.));
#5247=DIRECTION('ref_axis',(0.,0.,1.));
#5248=DIRECTION('center_axis',(0.,-1.,0.));
#5249=DIRECTION('ref_axis',(1.,0.,0.));
#5250=DIRECTION('center_axis',(0.,-1.,0.));
#5251=DIRECTION('ref_axis',(1.,0.,0.));
#5252=DIRECTION('center_axis',(0.,-1.,0.));
#5253=DIRECTION('ref_axis',(1.,0.,0.));
#5254=DIRECTION('',(0.707106781186548,0.707106781186547,8.65956056235493E-17));
#5255=DIRECTION('center_axis',(0.,-1.,0.));
#5256=DIRECTION('ref_axis',(1.,0.,0.));
#5257=DIRECTION('center_axis',(0.,-1.,0.));
#5258=DIRECTION('ref_axis',(1.,0.,0.));
#5259=DIRECTION('',(0.,1.,0.));
#5260=DIRECTION('center_axis',(0.,1.,0.));
#5261=DIRECTION('ref_axis',(1.,0.,0.));
#5262=DIRECTION('center_axis',(0.,-1.,0.));
#5263=DIRECTION('ref_axis',(1.,0.,0.));
#5264=DIRECTION('',(-0.707106781186547,0.707106781186548,-8.65956056235493E-17));
#5265=DIRECTION('center_axis',(0.,-1.,0.));
#5266=DIRECTION('ref_axis',(0.,0.,-1.));
#5267=DIRECTION('center_axis',(0.,-1.,0.));
#5268=DIRECTION('ref_axis',(1.,0.,0.));
#5269=DIRECTION('center_axis',(0.,1.,0.));
#5270=DIRECTION('ref_axis',(1.,0.,0.));
#5271=DIRECTION('center_axis',(0.,1.,0.));
#5272=DIRECTION('ref_axis',(1.,0.,0.));
#5273=DIRECTION('',(-0.447213595499958,0.894427190999916,-5.47678698264203E-17));
#5274=DIRECTION('center_axis',(0.,-1.,0.));
#5275=DIRECTION('ref_axis',(1.,0.,0.));
#5276=DIRECTION('',(0.,1.,0.));
#5277=DIRECTION('axis',(0.,0.,1.));
#5278=DIRECTION('refdir',(1.,0.,0.));
#5279=DIRECTION('center_axis',(0.,1.,0.));
#5280=DIRECTION('ref_axis',(0.,0.,1.));
#5281=DIRECTION('center_axis',(0.,-1.,0.));
#5282=DIRECTION('ref_axis',(1.,0.,0.));
#5283=DIRECTION('center_axis',(0.,-1.,0.));
#5284=DIRECTION('ref_axis',(1.,0.,0.));
#5285=DIRECTION('center_axis',(0.,-1.,0.));
#5286=DIRECTION('ref_axis',(1.,0.,0.));
#5287=DIRECTION('',(0.707106781186548,0.707106781186547,8.65956056235493E-17));
#5288=DIRECTION('center_axis',(0.,-1.,0.));
#5289=DIRECTION('ref_axis',(1.,0.,0.));
#5290=DIRECTION('center_axis',(0.,-1.,0.));
#5291=DIRECTION('ref_axis',(1.,0.,0.));
#5292=DIRECTION('',(0.,1.,0.));
#5293=DIRECTION('center_axis',(0.,1.,0.));
#5294=DIRECTION('ref_axis',(1.,0.,0.));
#5295=DIRECTION('center_axis',(0.,-1.,0.));
#5296=DIRECTION('ref_axis',(1.,0.,0.));
#5297=DIRECTION('',(-0.707106781186547,0.707106781186548,-8.65956056235493E-17));
#5298=DIRECTION('center_axis',(0.,-1.,0.));
#5299=DIRECTION('ref_axis',(0.,0.,-1.));
#5300=DIRECTION('center_axis',(0.,-1.,0.));
#5301=DIRECTION('ref_axis',(1.,0.,0.));
#5302=DIRECTION('center_axis',(0.,1.,0.));
#5303=DIRECTION('ref_axis',(1.,0.,0.));
#5304=DIRECTION('center_axis',(0.,1.,0.));
#5305=DIRECTION('ref_axis',(1.,0.,0.));
#5306=DIRECTION('',(-0.447213595499958,0.894427190999916,-5.47678698264203E-17));
#5307=DIRECTION('center_axis',(0.,-1.,0.));
#5308=DIRECTION('ref_axis',(1.,0.,0.));
#5309=DIRECTION('center_axis',(0.,1.,0.));
#5310=DIRECTION('ref_axis',(1.,0.,0.));
#5311=DIRECTION('',(0.,1.,0.));
#5312=DIRECTION('center_axis',(0.,1.,0.));
#5313=DIRECTION('ref_axis',(1.,0.,0.));
#5314=DIRECTION('center_axis',(0.,-1.,0.));
#5315=DIRECTION('ref_axis',(1.,0.,0.));
#5316=DIRECTION('',(-0.707106781186547,0.707106781186548,-8.65956056235493E-17));
#5317=DIRECTION('center_axis',(0.,-1.,0.));
#5318=DIRECTION('ref_axis',(0.,0.,-1.));
#5319=DIRECTION('center_axis',(0.866025403784439,0.,-0.5));
#5320=DIRECTION('ref_axis',(0.5,0.,0.866025403784439));
#5321=DIRECTION('',(-0.5,0.,-0.866025403784439));
#5322=DIRECTION('',(0.,-1.,0.));
#5323=DIRECTION('',(0.5,0.,0.866025403784439));
#5324=DIRECTION('',(0.,-1.,0.));
#5325=DIRECTION('center_axis',(1.20185167898973E-16,0.,-1.));
#5326=DIRECTION('ref_axis',(1.,0.,1.20185167898973E-16));
#5327=DIRECTION('',(-1.,0.,-1.20185167898973E-16));
#5328=DIRECTION('',(0.,-1.,0.));
#5329=DIRECTION('',(1.,0.,1.20185167898973E-16));
#5330=DIRECTION('center_axis',(-0.866025403784439,0.,-0.5));
#5331=DIRECTION('ref_axis',(0.5,0.,-0.866025403784439));
#5332=DIRECTION('',(-0.5,0.,0.866025403784439));
#5333=DIRECTION('',(0.,-1.,0.));
#5334=DIRECTION('',(0.5,0.,-0.866025403784439));
#5335=DIRECTION('center_axis',(-0.866025403784439,0.,0.5));
#5336=DIRECTION('ref_axis',(-0.5,0.,-0.866025403784439));
#5337=DIRECTION('',(0.5,0.,0.866025403784439));
#5338=DIRECTION('',(0.,-1.,0.));
#5339=DIRECTION('',(-0.5,0.,-0.866025403784439));
#5340=DIRECTION('center_axis',(-2.40370335797945E-16,0.,1.));
#5341=DIRECTION('ref_axis',(-1.,0.,-2.40370335797945E-16));
#5342=DIRECTION('',(1.,0.,2.40370335797945E-16));
#5343=DIRECTION('',(0.,-1.,0.));
#5344=DIRECTION('',(-1.,0.,-2.40370335797945E-16));
#5345=DIRECTION('center_axis',(0.866025403784439,0.,0.5));
#5346=DIRECTION('ref_axis',(-0.5,0.,0.866025403784439));
#5347=DIRECTION('',(0.5,0.,-0.866025403784439));
#5348=DIRECTION('',(-0.5,0.,0.866025403784439));
#5349=DIRECTION('center_axis',(0.,1.,0.));
#5350=DIRECTION('ref_axis',(1.,0.,0.));
#5351=DIRECTION('center_axis',(0.,-1.,0.));
#5352=DIRECTION('ref_axis',(0.,0.,-1.));
#5353=DIRECTION('axis',(0.,0.,1.));
#5354=DIRECTION('refdir',(1.,0.,0.));
#5355=DIRECTION('center_axis',(0.,1.,0.));
#5356=DIRECTION('ref_axis',(1.,0.,0.));
#5357=DIRECTION('center_axis',(-0.707106781186548,0.707106781186548,0.));
#5358=DIRECTION('ref_axis',(0.707106781186547,0.707106781186547,0.));
#5359=DIRECTION('center_axis',(0.,1.,0.));
#5360=DIRECTION('ref_axis',(1.,0.,0.));
#5361=DIRECTION('',(0.,1.,0.));
#5362=DIRECTION('center_axis',(0.,-1.,0.));
#5363=DIRECTION('ref_axis',(1.,0.,0.));
#5364=DIRECTION('center_axis',(0.,1.,0.));
#5365=DIRECTION('ref_axis',(1.,0.,0.));
#5366=DIRECTION('center_axis',(6.12323399573677E-17,0.,1.));
#5367=DIRECTION('ref_axis',(1.,0.,0.));
#5368=DIRECTION('center_axis',(-1.22464679914735E-16,1.,0.));
#5369=DIRECTION('ref_axis',(-1.,-1.22464679914735E-16,0.));
#5370=DIRECTION('center_axis',(1.,0.,0.));
#5371=DIRECTION('ref_axis',(0.,0.,-1.));
#5372=DIRECTION('center_axis',(1.,0.,0.));
#5373=DIRECTION('ref_axis',(0.,0.,-1.));
#5374=DIRECTION('center_axis',(1.,0.,0.));
#5375=DIRECTION('ref_axis',(0.,0.,-1.));
#5376=DIRECTION('',(1.,0.,0.));
#5377=DIRECTION('center_axis',(-1.,0.,0.));
#5378=DIRECTION('ref_axis',(0.,0.,-1.));
#5379=DIRECTION('center_axis',(0.,-1.,0.));
#5380=DIRECTION('ref_axis',(0.,0.,-1.));
#5381=DIRECTION('center_axis',(0.,-1.,0.));
#5382=DIRECTION('ref_axis',(1.,0.,0.));
#5383=DIRECTION('center_axis',(0.,-1.,0.));
#5384=DIRECTION('ref_axis',(1.,0.,0.));
#5385=DIRECTION('center_axis',(0.,-1.,0.));
#5386=DIRECTION('ref_axis',(1.,0.,0.));
#5387=DIRECTION('',(0.,-1.,0.));
#5388=DIRECTION('center_axis',(1.,0.,0.));
#5389=DIRECTION('ref_axis',(0.,1.,0.));
#5390=DIRECTION('center_axis',(1.,0.,0.));
#5391=DIRECTION('ref_axis',(0.,0.,-1.));
#5392=DIRECTION('',(1.,0.,0.));
#5393=DIRECTION('center_axis',(-1.,0.,0.));
#5394=DIRECTION('ref_axis',(0.,1.,0.));
#5395=DIRECTION('center_axis',(-1.,0.,0.));
#5396=DIRECTION('ref_axis',(0.,0.,1.));
#5397=DIRECTION('center_axis',(6.12323399573677E-17,0.,1.));
#5398=DIRECTION('ref_axis',(1.,0.,0.));
#5399=DIRECTION('center_axis',(0.,-1.,0.));
#5400=DIRECTION('ref_axis',(1.,0.,0.));
#5401=DIRECTION('center_axis',(0.,-1.,0.));
#5402=DIRECTION('ref_axis',(1.,0.,0.));
#5403=DIRECTION('center_axis',(1.,0.,0.));
#5404=DIRECTION('ref_axis',(0.,0.,-1.));
#5405=DIRECTION('center_axis',(1.,0.,0.));
#5406=DIRECTION('ref_axis',(0.,0.,-1.));
#5407=DIRECTION('center_axis',(0.,-1.,0.));
#5408=DIRECTION('ref_axis',(1.,0.,0.));
#5409=DIRECTION('center_axis',(0.707106781186548,-0.707106781186548,0.));
#5410=DIRECTION('ref_axis',(0.707106781186547,0.707106781186547,0.));
#5411=DIRECTION('',(0.,1.,0.));
#5412=DIRECTION('center_axis',(0.,-1.,0.));
#5413=DIRECTION('ref_axis',(1.,0.,0.));
#5414=DIRECTION('center_axis',(0.,1.,0.));
#5415=DIRECTION('ref_axis',(0.,0.,1.));
#5416=DIRECTION('center_axis',(0.,-1.,0.));
#5417=DIRECTION('ref_axis',(1.,0.,0.));
#5418=DIRECTION('center_axis',(0.,-1.,0.));
#5419=DIRECTION('ref_axis',(1.,0.,0.));
#5420=DIRECTION('center_axis',(0.,-1.,0.));
#5421=DIRECTION('ref_axis',(1.,0.,0.));
#5422=DIRECTION('',(0.,1.,0.));
#5423=DIRECTION('center_axis',(0.,-1.,0.));
#5424=DIRECTION('ref_axis',(0.,0.,-1.));
#5425=DIRECTION('center_axis',(-1.,0.,0.));
#5426=DIRECTION('ref_axis',(0.,0.,1.));
#5427=DIRECTION('center_axis',(1.,0.,0.));
#5428=DIRECTION('ref_axis',(0.,0.,-1.));
#5429=DIRECTION('center_axis',(1.,0.,0.));
#5430=DIRECTION('ref_axis',(0.,0.,-1.));
#5431=DIRECTION('center_axis',(1.,0.,0.));
#5432=DIRECTION('ref_axis',(0.,1.,0.));
#5433=DIRECTION('center_axis',(1.,0.,0.));
#5434=DIRECTION('ref_axis',(0.,0.,-1.));
#5435=DIRECTION('',(-1.,0.,0.));
#5436=DIRECTION('center_axis',(1.,0.,0.));
#5437=DIRECTION('ref_axis',(0.,0.,-1.));
#5438=DIRECTION('center_axis',(1.,0.,0.));
#5439=DIRECTION('ref_axis',(0.,1.,0.));
#5440=DIRECTION('',(-1.,0.,0.));
#5441=DIRECTION('axis',(0.,0.,1.));
#5442=DIRECTION('refdir',(1.,0.,0.));
#5443=DIRECTION('center_axis',(0.,1.,0.));
#5444=DIRECTION('ref_axis',(1.,0.,0.));
#5445=DIRECTION('',(-0.5,0.,0.866025403784439));
#5446=DIRECTION('',(-1.,0.,-2.84883360945713E-16));
#5447=DIRECTION('',(-0.5,0.,-0.866025403784439));
#5448=DIRECTION('',(0.5,0.,-0.866025403784439));
#5449=DIRECTION('',(1.,0.,0.));
#5450=DIRECTION('',(0.5,0.,0.866025403784439));
#5451=DIRECTION('center_axis',(0.,-1.,0.));
#5452=DIRECTION('ref_axis',(1.,0.,0.));
#5453=DIRECTION('center_axis',(0.,1.,0.));
#5454=DIRECTION('ref_axis',(1.,0.,0.));
#5455=DIRECTION('',(0.5,0.,-0.866025403784439));
#5456=DIRECTION('',(-0.5,0.,-0.866025403784439));
#5457=DIRECTION('',(-1.,0.,0.));
#5458=DIRECTION('',(-0.5,0.,0.866025403784439));
#5459=DIRECTION('',(0.5,0.,0.866025403784439));
#5460=DIRECTION('',(1.,0.,2.84883360945713E-16));
#5461=DIRECTION('center_axis',(0.,1.,0.));
#5462=DIRECTION('ref_axis',(1.,0.,0.));
#5463=DIRECTION('center_axis',(-2.84883360945713E-16,0.,1.));
#5464=DIRECTION('ref_axis',(1.,0.,2.84883360945713E-16));
#5465=DIRECTION('',(0.,-1.,0.));
#5466=DIRECTION('',(0.,1.,0.));
#5467=DIRECTION('center_axis',(-0.866025403784439,0.,0.5));
#5468=DIRECTION('ref_axis',(0.5,0.,0.866025403784439));
#5469=DIRECTION('',(0.,1.,0.));
#5470=DIRECTION('center_axis',(-0.866025403784439,0.,-0.5));
#5471=DIRECTION('ref_axis',(-0.5,0.,0.866025403784439));
#5472=DIRECTION('',(0.,1.,0.));
#5473=DIRECTION('center_axis',(0.,0.,-1.));
#5474=DIRECTION('ref_axis',(-1.,0.,0.));
#5475=DIRECTION('',(0.,1.,0.));
#5476=DIRECTION('center_axis',(0.866025403784439,0.,-0.5));
#5477=DIRECTION('ref_axis',(-0.5,0.,-0.866025403784439));
#5478=DIRECTION('',(0.,1.,0.));
#5479=DIRECTION('center_axis',(0.866025403784439,0.,0.5));
#5480=DIRECTION('ref_axis',(0.5,0.,-0.866025403784439));
#5481=DIRECTION('center_axis',(0.,-1.,0.));
#5482=DIRECTION('ref_axis',(1.,0.,0.));
#5483=DIRECTION('',(0.,1.,0.));
#5484=DIRECTION('center_axis',(0.,-1.,0.));
#5485=DIRECTION('ref_axis',(1.,0.,0.));
#5486=DIRECTION('center_axis',(0.,1.,0.));
#5487=DIRECTION('ref_axis',(0.,0.,1.));
#5488=DIRECTION('center_axis',(0.,-1.,0.));
#5489=DIRECTION('ref_axis',(1.,0.,0.));
#5490=DIRECTION('center_axis',(0.,-1.,0.));
#5491=DIRECTION('ref_axis',(1.,0.,0.));
#5492=DIRECTION('center_axis',(0.,-1.,0.));
#5493=DIRECTION('ref_axis',(1.,0.,0.));
#5494=DIRECTION('',(0.707106781186547,0.707106781186548,8.65956056235493E-17));
#5495=DIRECTION('center_axis',(0.,-1.,0.));
#5496=DIRECTION('ref_axis',(1.,0.,0.));
#5497=DIRECTION('center_axis',(0.,-1.,0.));
#5498=DIRECTION('ref_axis',(1.,0.,0.));
#5499=DIRECTION('',(0.,1.,0.));
#5500=DIRECTION('center_axis',(0.,1.,0.));
#5501=DIRECTION('ref_axis',(1.,0.,0.));
#5502=DIRECTION('center_axis',(0.,-1.,0.));
#5503=DIRECTION('ref_axis',(1.,0.,0.));
#5504=DIRECTION('',(-0.707106781186547,0.707106781186548,-8.65956056235493E-17));
#5505=DIRECTION('center_axis',(0.,-1.,0.));
#5506=DIRECTION('ref_axis',(0.,0.,-1.));
#5507=DIRECTION('center_axis',(0.,-1.,0.));
#5508=DIRECTION('ref_axis',(1.,0.,0.));
#5509=DIRECTION('center_axis',(0.,-1.,0.));
#5510=DIRECTION('ref_axis',(1.,0.,0.));
#5511=DIRECTION('',(0.,1.,0.));
#5512=DIRECTION('axis',(0.,0.,1.));
#5513=DIRECTION('refdir',(1.,0.,0.));
#5514=DIRECTION('center_axis',(0.,1.,0.));
#5515=DIRECTION('ref_axis',(0.,0.,1.));
#5516=DIRECTION('center_axis',(0.,-1.,0.));
#5517=DIRECTION('ref_axis',(1.,0.,0.));
#5518=DIRECTION('center_axis',(0.,-1.,0.));
#5519=DIRECTION('ref_axis',(1.,0.,0.));
#5520=DIRECTION('center_axis',(0.,-1.,0.));
#5521=DIRECTION('ref_axis',(1.,0.,0.));
#5522=DIRECTION('',(0.707106781186548,0.707106781186547,8.65956056235493E-17));
#5523=DIRECTION('center_axis',(0.,-1.,0.));
#5524=DIRECTION('ref_axis',(1.,0.,0.));
#5525=DIRECTION('center_axis',(0.,-1.,0.));
#5526=DIRECTION('ref_axis',(1.,0.,0.));
#5527=DIRECTION('',(0.,1.,0.));
#5528=DIRECTION('center_axis',(0.,1.,0.));
#5529=DIRECTION('ref_axis',(1.,0.,0.));
#5530=DIRECTION('center_axis',(0.,-1.,0.));
#5531=DIRECTION('ref_axis',(1.,0.,0.));
#5532=DIRECTION('',(-0.707106781186548,0.707106781186547,-8.65956056235494E-17));
#5533=DIRECTION('center_axis',(0.,-1.,0.));
#5534=DIRECTION('ref_axis',(0.,0.,-1.));
#5535=DIRECTION('center_axis',(0.,-1.,0.));
#5536=DIRECTION('ref_axis',(1.,0.,0.));
#5537=DIRECTION('center_axis',(0.,1.,0.));
#5538=DIRECTION('ref_axis',(1.,0.,0.));
#5539=DIRECTION('center_axis',(0.,1.,0.));
#5540=DIRECTION('ref_axis',(1.,0.,0.));
#5541=DIRECTION('',(-0.447213595499958,0.894427190999916,-5.47678698264203E-17));
#5542=DIRECTION('center_axis',(0.,-1.,0.));
#5543=DIRECTION('ref_axis',(1.,0.,0.));
#5544=DIRECTION('center_axis',(0.,1.,0.));
#5545=DIRECTION('ref_axis',(1.,0.,0.));
#5546=DIRECTION('',(0.,1.,0.));
#5547=DIRECTION('center_axis',(0.,1.,0.));
#5548=DIRECTION('ref_axis',(1.,0.,0.));
#5549=DIRECTION('center_axis',(0.,-1.,0.));
#5550=DIRECTION('ref_axis',(1.,0.,0.));
#5551=DIRECTION('',(-0.707106781186547,0.707106781186548,-8.65956056235493E-17));
#5552=DIRECTION('center_axis',(0.,-1.,0.));
#5553=DIRECTION('ref_axis',(0.,0.,-1.));
#5554=DIRECTION('center_axis',(0.866025403784439,0.,-0.5));
#5555=DIRECTION('ref_axis',(0.5,0.,0.866025403784439));
#5556=DIRECTION('',(-0.5,0.,-0.866025403784439));
#5557=DIRECTION('',(0.,-1.,0.));
#5558=DIRECTION('',(0.5,0.,0.866025403784439));
#5559=DIRECTION('',(0.,-1.,0.));
#5560=DIRECTION('center_axis',(1.60246890531964E-16,0.,-1.));
#5561=DIRECTION('ref_axis',(1.,0.,1.60246890531964E-16));
#5562=DIRECTION('',(-1.,0.,-1.60246890531964E-16));
#5563=DIRECTION('',(0.,-1.,0.));
#5564=DIRECTION('',(1.,0.,1.60246890531964E-16));
#5565=DIRECTION('center_axis',(-0.866025403784439,0.,-0.5));
#5566=DIRECTION('ref_axis',(0.5,0.,-0.866025403784439));
#5567=DIRECTION('',(-0.5,0.,0.866025403784439));
#5568=DIRECTION('',(0.,-1.,0.));
#5569=DIRECTION('',(0.5,0.,-0.866025403784439));
#5570=DIRECTION('center_axis',(-0.866025403784439,0.,0.5));
#5571=DIRECTION('ref_axis',(-0.5,0.,-0.866025403784439));
#5572=DIRECTION('',(0.5,0.,0.866025403784439));
#5573=DIRECTION('',(0.,-1.,0.));
#5574=DIRECTION('',(-0.5,0.,-0.866025403784439));
#5575=DIRECTION('center_axis',(-1.60246890531964E-16,0.,1.));
#5576=DIRECTION('ref_axis',(-1.,0.,-1.60246890531964E-16));
#5577=DIRECTION('',(1.,0.,1.60246890531964E-16));
#5578=DIRECTION('',(0.,-1.,0.));
#5579=DIRECTION('',(-1.,0.,-1.60246890531964E-16));
#5580=DIRECTION('center_axis',(0.866025403784439,0.,0.5));
#5581=DIRECTION('ref_axis',(-0.5,0.,0.866025403784439));
#5582=DIRECTION('',(0.5,0.,-0.866025403784439));
#5583=DIRECTION('',(-0.5,0.,0.866025403784439));
#5584=DIRECTION('center_axis',(0.,1.,0.));
#5585=DIRECTION('ref_axis',(1.,0.,0.));
#5586=DIRECTION('center_axis',(0.,-1.,0.));
#5587=DIRECTION('ref_axis',(0.,0.,-1.));
#5588=DIRECTION('axis',(0.,0.,1.));
#5589=DIRECTION('refdir',(1.,0.,0.));
#5590=DIRECTION('center_axis',(0.,1.,0.));
#5591=DIRECTION('ref_axis',(1.,0.,0.));
#5592=DIRECTION('center_axis',(0.,-1.,0.));
#5593=DIRECTION('ref_axis',(1.,0.,0.));
#5594=DIRECTION('',(0.,-1.,0.));
#5595=DIRECTION('center_axis',(0.,-1.,0.));
#5596=DIRECTION('ref_axis',(1.,0.,0.));
#5597=DIRECTION('center_axis',(0.,1.,0.));
#5598=DIRECTION('ref_axis',(1.,0.,0.));
#5599=DIRECTION('center_axis',(0.,1.,0.));
#5600=DIRECTION('ref_axis',(1.,0.,0.));
#5601=DIRECTION('',(0.,-1.,0.));
#5602=DIRECTION('center_axis',(0.,1.,0.));
#5603=DIRECTION('ref_axis',(1.,0.,0.));
#5604=DIRECTION('center_axis',(0.,1.,0.));
#5605=DIRECTION('ref_axis',(1.,0.,0.));
#5606=DIRECTION('center_axis',(0.,1.,0.));
#5607=DIRECTION('ref_axis',(1.,0.,0.));
#5608=DIRECTION('axis',(0.,0.,1.));
#5609=DIRECTION('refdir',(1.,0.,0.));
#5610=DIRECTION('center_axis',(0.,1.,0.));
#5611=DIRECTION('ref_axis',(1.,0.,0.));
#5612=DIRECTION('',(0.866025403784439,-0.5,1.06057523872491E-16));
#5613=DIRECTION('center_axis',(0.,-1.,0.));
#5614=DIRECTION('ref_axis',(1.,0.,0.));
#5615=DIRECTION('center_axis',(0.,-1.,0.));
#5616=DIRECTION('ref_axis',(1.,0.,0.));
#5617=DIRECTION('center_axis',(0.,1.,0.));
#5618=DIRECTION('ref_axis',(1.,0.,0.));
#5619=DIRECTION('',(-0.866025403784439,-0.5,-1.06057523872491E-16));
#5620=DIRECTION('center_axis',(1.4792020664489E-16,0.,-1.));
#5621=DIRECTION('ref_axis',(-1.,0.,-1.4792020664489E-16));
#5622=DIRECTION('',(0.,1.,0.));
#5623=DIRECTION('',(0.,1.,0.));
#5624=DIRECTION('center_axis',(-0.866025403784439,0.,-0.5));
#5625=DIRECTION('ref_axis',(-0.5,0.,0.866025403784439));
#5626=DIRECTION('',(0.,1.,0.));
#5627=DIRECTION('center_axis',(-0.866025403784439,0.,0.5));
#5628=DIRECTION('ref_axis',(0.5,0.,0.866025403784439));
#5629=DIRECTION('',(0.,1.,0.));
#5630=DIRECTION('center_axis',(0.,1.,0.));
#5631=DIRECTION('ref_axis',(1.,0.,0.));
#5632=DIRECTION('center_axis',(0.,1.,0.));
#5633=DIRECTION('ref_axis',(1.,0.,0.));
#5634=DIRECTION('',(0.,-1.,0.));
#5635=DIRECTION('center_axis',(0.,1.,0.));
#5636=DIRECTION('ref_axis',(1.,0.,0.));
#5637=DIRECTION('center_axis',(-2.95840413289779E-16,0.,1.));
#5638=DIRECTION('ref_axis',(1.,0.,2.95840413289779E-16));
#5639=DIRECTION('',(0.,1.,0.));
#5640=DIRECTION('center_axis',(0.866025403784439,0.,-0.5));
#5641=DIRECTION('ref_axis',(-0.5,0.,-0.866025403784439));
#5642=DIRECTION('',(0.,1.,0.));
#5643=DIRECTION('center_axis',(0.866025403784439,0.,0.5));
#5644=DIRECTION('ref_axis',(0.5,0.,-0.866025403784439));
#5645=DIRECTION('center_axis',(0.,1.,0.));
#5646=DIRECTION('ref_axis',(1.,0.,0.));
#5647=DIRECTION('center_axis',(0.,1.,0.));
#5648=DIRECTION('ref_axis',(1.,0.,0.));
#5649=DIRECTION('',(0.,0.,1.));
#5650=DIRECTION('',(1.,0.,0.));
#5651=DIRECTION('',(0.,0.,1.));
#5652=DIRECTION('',(1.,0.,0.));
#5653=DIRECTION('',(0.,0.,1.));
#5654=DIRECTION('',(1.,0.,0.));
#5655=DIRECTION('',(0.,0.,1.));
#5656=DIRECTION('',(1.,0.,0.));
#5657=DIRECTION('',(0.,0.,1.));
#5658=DIRECTION('',(1.,0.,0.));
#5659=DIRECTION('',(0.,0.,1.));
#5660=DIRECTION('',(1.,0.,0.));
#5661=DIRECTION('',(0.,0.,1.));
#5662=DIRECTION('',(1.,0.,0.));
#5663=DIRECTION('',(0.,0.,1.));
#5664=DIRECTION('',(1.,0.,0.));
#5665=DIRECTION('',(0.,0.,1.));
#5666=DIRECTION('',(1.,0.,0.));
#5667=DIRECTION('',(0.,0.,1.));
#5668=DIRECTION('',(1.,0.,0.));
#5669=DIRECTION('',(0.,0.,1.));
#5670=DIRECTION('',(1.,0.,0.));
#5671=DIRECTION('',(0.,0.,1.));
#5672=DIRECTION('',(1.,0.,0.));
#5673=DIRECTION('',(0.,-1.,2.22044604925031E-16));
#5674=DIRECTION('',(1.,0.,0.));
#5675=DIRECTION('',(0.,-1.,2.22044604925031E-16));
#5676=DIRECTION('',(1.,0.,0.));
#5677=DIRECTION('',(0.,-1.,2.22044604925031E-16));
#5678=DIRECTION('',(1.,0.,0.));
#5679=DIRECTION('',(0.,-1.,2.22044604925031E-16));
#5680=DIRECTION('',(1.,0.,0.));
#5681=DIRECTION('',(0.,-1.,2.22044604925031E-16));
#5682=DIRECTION('',(1.,0.,0.));
#5683=DIRECTION('',(0.,-1.,2.22044604925031E-16));
#5684=DIRECTION('',(1.,0.,0.));
#5685=DIRECTION('',(0.,-1.,2.22044604925031E-16));
#5686=DIRECTION('',(1.,0.,0.));
#5687=DIRECTION('',(0.,-1.,2.22044604925031E-16));
#5688=DIRECTION('',(1.,0.,0.));
#5689=DIRECTION('',(0.,0.,1.));
#5690=DIRECTION('',(1.,0.,0.));
#5691=DIRECTION('',(0.,0.,1.));
#5692=DIRECTION('',(-1.,1.22464679914735E-16,0.));
#5693=DIRECTION('',(0.,0.,1.));
#5694=DIRECTION('',(2.22044604925031E-16,-1.,0.));
#5695=DIRECTION('',(0.,0.,1.));
#5696=DIRECTION('',(2.22044604925031E-16,-1.,0.));
#5697=DIRECTION('',(0.,0.,1.));
#5698=DIRECTION('',(2.22044604925031E-16,-1.,0.));
#5699=DIRECTION('',(0.,0.,1.));
#5700=DIRECTION('',(2.22044604925031E-16,1.,0.));
#5701=DIRECTION('',(0.,0.,1.));
#5702=DIRECTION('',(2.22044604925031E-16,-1.,0.));
#5703=DIRECTION('',(0.,0.,1.));
#5704=DIRECTION('',(2.22044604925031E-16,-1.,0.));
#5705=DIRECTION('',(0.,0.,1.));
#5706=DIRECTION('',(2.22044604925031E-16,-1.,0.));
#5707=DIRECTION('',(0.,0.,1.));
#5708=DIRECTION('',(2.22044604925031E-16,1.,0.));
#5709=DIRECTION('',(0.,0.,1.));
#5710=DIRECTION('',(2.22044604925031E-16,-1.,0.));
#5711=DIRECTION('',(0.,0.,1.));
#5712=DIRECTION('',(2.22044604925031E-16,-1.,0.));
#5713=DIRECTION('',(0.,0.,1.));
#5714=DIRECTION('',(2.22044604925031E-16,-1.,0.));
#5715=DIRECTION('',(0.,0.,1.));
#5716=DIRECTION('',(2.22044604925031E-16,1.,0.));
#5717=DIRECTION('',(0.,0.,1.));
#5718=DIRECTION('',(2.22044604925031E-16,-1.,0.));
#5719=DIRECTION('',(0.,0.,1.));
#5720=DIRECTION('',(2.22044604925031E-16,-1.,0.));
#5721=DIRECTION('',(0.,0.,1.));
#5722=DIRECTION('',(2.22044604925031E-16,-1.,0.));
#5723=DIRECTION('',(0.,0.,1.));
#5724=DIRECTION('',(2.22044604925031E-16,1.,0.));
#5725=DIRECTION('',(0.,0.,1.));
#5726=DIRECTION('',(2.22044604925031E-16,-1.,0.));
#5727=DIRECTION('',(0.,0.,1.));
#5728=DIRECTION('',(2.22044604925031E-16,-1.,0.));
#5729=CARTESIAN_POINT('',(0.,0.,0.));
#5730=CARTESIAN_POINT('',(0.,0.,0.));
#5731=CARTESIAN_POINT('Origin',(4.5,-2.6,-0.1));
#5732=CARTESIAN_POINT('',(4.29,-2.6,0.));
#5733=CARTESIAN_POINT('Origin',(4.5,-2.6,0.));
#5734=CARTESIAN_POINT('',(4.29,-2.6,1.));
#5735=CARTESIAN_POINT('',(4.29,-2.6,-0.1));
#5736=CARTESIAN_POINT('Origin',(4.5,-2.6,1.));
#5737=CARTESIAN_POINT('Origin',(-4.5,2.6,-0.1));
#5738=CARTESIAN_POINT('',(-4.71,2.6,0.));
#5739=CARTESIAN_POINT('Origin',(-4.5,2.6,0.));
#5740=CARTESIAN_POINT('',(-4.71,2.6,1.));
#5741=CARTESIAN_POINT('',(-4.71,2.6,-0.1));
#5742=CARTESIAN_POINT('Origin',(-4.5,2.6,1.));
#5743=CARTESIAN_POINT('Origin',(-4.5,-2.6,-0.1));
#5744=CARTESIAN_POINT('',(-4.71,-2.6,0.));
#5745=CARTESIAN_POINT('Origin',(-4.5,-2.6,0.));
#5746=CARTESIAN_POINT('',(-4.71,-2.6,1.));
#5747=CARTESIAN_POINT('',(-4.71,-2.6,-0.1));
#5748=CARTESIAN_POINT('Origin',(-4.5,-2.6,1.));
#5749=CARTESIAN_POINT('Origin',(4.5,2.6,-0.1));
#5750=CARTESIAN_POINT('',(4.29,2.6,0.));
#5751=CARTESIAN_POINT('Origin',(4.5,2.6,0.));
#5752=CARTESIAN_POINT('',(4.29,2.6,1.));
#5753=CARTESIAN_POINT('',(4.29,2.6,-0.1));
#5754=CARTESIAN_POINT('Origin',(4.5,2.6,1.));
#5755=CARTESIAN_POINT('Origin',(14.,5.,0.));
#5756=CARTESIAN_POINT('',(14.,5.,0.));
#5757=CARTESIAN_POINT('',(-14.,5.,0.));
#5758=CARTESIAN_POINT('',(14.,5.,0.));
#5759=CARTESIAN_POINT('',(-14.,5.,1.));
#5760=CARTESIAN_POINT('',(-14.,5.,0.));
#5761=CARTESIAN_POINT('',(14.,5.,1.));
#5762=CARTESIAN_POINT('',(14.,5.,1.));
#5763=CARTESIAN_POINT('',(14.,5.,0.));
#5764=CARTESIAN_POINT('Origin',(14.,-5.,0.));
#5765=CARTESIAN_POINT('',(14.,-5.,0.));
#5766=CARTESIAN_POINT('',(14.,-5.,0.));
#5767=CARTESIAN_POINT('',(14.,-5.,1.));
#5768=CARTESIAN_POINT('',(14.,-5.,1.));
#5769=CARTESIAN_POINT('',(14.,-5.,0.));
#5770=CARTESIAN_POINT('Origin',(-14.,-5.,0.));
#5771=CARTESIAN_POINT('',(-14.,-5.,0.));
#5772=CARTESIAN_POINT('',(-14.,-5.,0.));
#5773=CARTESIAN_POINT('',(-14.,-5.,1.));
#5774=CARTESIAN_POINT('',(-14.,-5.,1.));
#5775=CARTESIAN_POINT('',(-14.,-5.,0.));
#5776=CARTESIAN_POINT('Origin',(-14.,5.,0.));
#5777=CARTESIAN_POINT('',(-14.,5.,0.));
#5778=CARTESIAN_POINT('',(-14.,5.,1.));
#5779=CARTESIAN_POINT('Origin',(0.,0.,1.));
#5780=CARTESIAN_POINT('Origin',(0.,0.,0.));
#5781=CARTESIAN_POINT('',(0.,0.,0.));
#5782=CARTESIAN_POINT('Origin',(-12.,5.,-0.3));
#5783=CARTESIAN_POINT('',(-12.,5.,-0.3));
#5784=CARTESIAN_POINT('',(-14.,5.,-0.3));
#5785=CARTESIAN_POINT('',(-12.,5.,-0.3));
#5786=CARTESIAN_POINT('',(-14.,5.,0.));
#5787=CARTESIAN_POINT('',(-14.,5.,-0.3));
#5788=CARTESIAN_POINT('',(-12.,5.,0.));
#5789=CARTESIAN_POINT('',(-12.,5.,0.));
#5790=CARTESIAN_POINT('',(-12.,5.,-0.3));
#5791=CARTESIAN_POINT('Origin',(-12.,-5.,-0.3));
#5792=CARTESIAN_POINT('',(-12.,-5.,-0.3));
#5793=CARTESIAN_POINT('',(-12.,-5.,-0.3));
#5794=CARTESIAN_POINT('',(-12.,-5.,0.));
#5795=CARTESIAN_POINT('',(-12.,-5.,0.));
#5796=CARTESIAN_POINT('',(-12.,-5.,-0.3));
#5797=CARTESIAN_POINT('Origin',(-14.,-5.,-0.3));
#5798=CARTESIAN_POINT('',(-14.,-5.,-0.3));
#5799=CARTESIAN_POINT('',(-14.,-5.,-0.3));
#5800=CARTESIAN_POINT('',(-14.,-5.,0.));
#5801=CARTESIAN_POINT('',(-14.,-5.,0.));
#5802=CARTESIAN_POINT('',(-14.,-5.,-0.3));
#5803=CARTESIAN_POINT('Origin',(-14.,5.,-0.3));
#5804=CARTESIAN_POINT('',(-14.,5.,-0.3));
#5805=CARTESIAN_POINT('',(-14.,5.,0.));
#5806=CARTESIAN_POINT('Origin',(-13.,0.,0.));
#5807=CARTESIAN_POINT('Origin',(-13.,0.,-0.3));
#5808=CARTESIAN_POINT('',(0.,0.,0.));
#5809=CARTESIAN_POINT('Origin',(14.,5.,-0.3));
#5810=CARTESIAN_POINT('',(14.,5.,-0.3));
#5811=CARTESIAN_POINT('',(12.,5.,-0.3));
#5812=CARTESIAN_POINT('',(14.,5.,-0.3));
#5813=CARTESIAN_POINT('',(12.,5.,0.));
#5814=CARTESIAN_POINT('',(12.,5.,-0.3));
#5815=CARTESIAN_POINT('',(14.,5.,0.));
#5816=CARTESIAN_POINT('',(14.,5.,0.));
#5817=CARTESIAN_POINT('',(14.,5.,-0.3));
#5818=CARTESIAN_POINT('Origin',(14.,-5.,-0.3));
#5819=CARTESIAN_POINT('',(14.,-5.,-0.3));
#5820=CARTESIAN_POINT('',(14.,-5.,-0.3));
#5821=CARTESIAN_POINT('',(14.,-5.,0.));
#5822=CARTESIAN_POINT('',(14.,-5.,0.));
#5823=CARTESIAN_POINT('',(14.,-5.,-0.3));
#5824=CARTESIAN_POINT('Origin',(12.,-5.,-0.3));
#5825=CARTESIAN_POINT('',(12.,-5.,-0.3));
#5826=CARTESIAN_POINT('',(12.,-5.,-0.3));
#5827=CARTESIAN_POINT('',(12.,-5.,0.));
#5828=CARTESIAN_POINT('',(12.,-5.,0.));
#5829=CARTESIAN_POINT('',(12.,-5.,-0.3));
#5830=CARTESIAN_POINT('Origin',(12.,5.,-0.3));
#5831=CARTESIAN_POINT('',(12.,5.,-0.3));
#5832=CARTESIAN_POINT('',(12.,5.,0.));
#5833=CARTESIAN_POINT('Origin',(13.,0.,0.));
#5834=CARTESIAN_POINT('Origin',(13.,0.,-0.3));
#5835=CARTESIAN_POINT('',(0.,0.,0.));
#5836=CARTESIAN_POINT('Origin',(-4.5,-2.,4.9));
#5837=CARTESIAN_POINT('',(-4.71,-2.,4.9));
#5838=CARTESIAN_POINT('Origin',(-4.5,-2.,4.9));
#5839=CARTESIAN_POINT('',(-4.71,-2.,6.));
#5840=CARTESIAN_POINT('',(-4.71,-2.,4.9));
#5841=CARTESIAN_POINT('Origin',(-4.5,-2.,6.));
#5842=CARTESIAN_POINT('Origin',(-4.5,-2.,4.9));
#5843=CARTESIAN_POINT('Origin',(-4.5,2.,4.9));
#5844=CARTESIAN_POINT('',(-4.71,2.,4.9));
#5845=CARTESIAN_POINT('Origin',(-4.5,2.,4.9));
#5846=CARTESIAN_POINT('',(-4.71,2.,6.));
#5847=CARTESIAN_POINT('',(-4.71,2.,4.9));
#5848=CARTESIAN_POINT('Origin',(-4.5,2.,6.));
#5849=CARTESIAN_POINT('Origin',(-4.5,2.,4.9));
#5850=CARTESIAN_POINT('Origin',(-4.5,-2.6,0.9));
#5851=CARTESIAN_POINT('',(-4.775,-2.6,1.));
#5852=CARTESIAN_POINT('Origin',(-4.5,-2.6,1.));
#5853=CARTESIAN_POINT('',(-4.775,-2.6,1.8));
#5854=CARTESIAN_POINT('',(-4.775,-2.6,0.9));
#5855=CARTESIAN_POINT('Origin',(-4.5,-2.6,1.8));
#5856=CARTESIAN_POINT('Origin',(-4.5,2.6,0.9));
#5857=CARTESIAN_POINT('',(-4.775,2.6,1.));
#5858=CARTESIAN_POINT('Origin',(-4.5,2.6,1.));
#5859=CARTESIAN_POINT('',(-4.775,2.6,1.8));
#5860=CARTESIAN_POINT('',(-4.775,2.6,0.9));
#5861=CARTESIAN_POINT('Origin',(-4.5,2.6,1.8));
#5862=CARTESIAN_POINT('Origin',(-5.2,0.,6.));
#5863=CARTESIAN_POINT('',(-3.9,-1.31,6.));
#5864=CARTESIAN_POINT('',(-5.1,-1.31,6.));
#5865=CARTESIAN_POINT('',(-5.2,-1.31,6.));
#5866=CARTESIAN_POINT('',(-3.9,1.31,6.));
#5867=CARTESIAN_POINT('Origin',(-3.9,0.,6.));
#5868=CARTESIAN_POINT('',(-5.1,1.31,6.));
#5869=CARTESIAN_POINT('',(-5.2,1.31,6.));
#5870=CARTESIAN_POINT('Origin',(-5.1,0.,6.));
#5871=CARTESIAN_POINT('Origin',(-3.9,0.,3.5));
#5872=CARTESIAN_POINT('',(-3.9,-2.4,6.));
#5873=CARTESIAN_POINT('',(-3.9,2.4,6.));
#5874=CARTESIAN_POINT('',(-3.9,-2.4,4.5));
#5875=CARTESIAN_POINT('',(-3.9,-2.4,6.));
#5876=CARTESIAN_POINT('',(-3.9,-1.,4.5));
#5877=CARTESIAN_POINT('',(-3.9,-2.4,4.5));
#5878=CARTESIAN_POINT('',(-3.9,-1.,1.8));
#5879=CARTESIAN_POINT('',(-3.9,-1.,4.5));
#5880=CARTESIAN_POINT('',(-3.9,-3.2,1.8));
#5881=CARTESIAN_POINT('',(-3.9,-1.,1.8));
#5882=CARTESIAN_POINT('',(-3.9,-3.2,1.));
#5883=CARTESIAN_POINT('',(-3.9,-3.2,1.8));
#5884=CARTESIAN_POINT('',(-3.9,3.2,1.));
#5885=CARTESIAN_POINT('',(-3.9,-3.2,1.));
#5886=CARTESIAN_POINT('',(-3.9,3.2,1.8));
#5887=CARTESIAN_POINT('',(-3.9,3.2,1.));
#5888=CARTESIAN_POINT('',(-3.9,1.,1.8));
#5889=CARTESIAN_POINT('',(-3.9,3.2,1.8));
#5890=CARTESIAN_POINT('',(-3.9,1.,4.5));
#5891=CARTESIAN_POINT('',(-3.9,1.,1.8));
#5892=CARTESIAN_POINT('',(-3.9,2.4,4.5));
#5893=CARTESIAN_POINT('',(-3.9,1.,4.5));
#5894=CARTESIAN_POINT('',(-3.9,2.4,6.));
#5895=CARTESIAN_POINT('',(-3.9,2.4,4.5));
#5896=CARTESIAN_POINT('',(-3.9,2.4,6.));
#5897=CARTESIAN_POINT('Origin',(-5.1,2.4,6.));
#5898=CARTESIAN_POINT('',(-5.1,-2.4,6.));
#5899=CARTESIAN_POINT('',(-5.1,2.4,6.));
#5900=CARTESIAN_POINT('',(-5.1,-2.4,6.));
#5901=CARTESIAN_POINT('Origin',(-5.1,2.4,6.));
#5902=CARTESIAN_POINT('',(-5.1,2.4,6.));
#5903=CARTESIAN_POINT('',(-5.1,2.4,6.));
#5904=CARTESIAN_POINT('',(-5.1,2.4,6.));
#5905=CARTESIAN_POINT('Origin',(-5.1,-1.,1.8));
#5906=CARTESIAN_POINT('',(-5.1,-1.,1.8));
#5907=CARTESIAN_POINT('',(-5.1,-3.2,1.8));
#5908=CARTESIAN_POINT('',(-5.1,-1.,1.8));
#5909=CARTESIAN_POINT('',(-5.1,-3.2,1.8));
#5910=CARTESIAN_POINT('',(-5.1,-1.,1.8));
#5911=CARTESIAN_POINT('Origin',(-5.1,-1.,4.5));
#5912=CARTESIAN_POINT('',(-5.1,-1.,4.5));
#5913=CARTESIAN_POINT('',(-5.1,-1.,4.5));
#5914=CARTESIAN_POINT('',(-5.1,-1.,4.5));
#5915=CARTESIAN_POINT('Origin',(-5.1,-2.4,4.5));
#5916=CARTESIAN_POINT('',(-5.1,-2.4,4.5));
#5917=CARTESIAN_POINT('',(-5.1,-2.4,4.5));
#5918=CARTESIAN_POINT('',(-5.1,-2.4,4.5));
#5919=CARTESIAN_POINT('Origin',(-5.1,-2.4,6.));
#5920=CARTESIAN_POINT('',(-5.1,-2.4,6.));
#5921=CARTESIAN_POINT('Origin',(-5.1,2.4,4.5));
#5922=CARTESIAN_POINT('',(-5.1,2.4,4.5));
#5923=CARTESIAN_POINT('',(-5.1,2.4,4.5));
#5924=CARTESIAN_POINT('',(-5.1,2.4,4.5));
#5925=CARTESIAN_POINT('Origin',(-5.1,1.,4.5));
#5926=CARTESIAN_POINT('',(-5.1,1.,4.5));
#5927=CARTESIAN_POINT('',(-5.1,1.,4.5));
#5928=CARTESIAN_POINT('',(-5.1,1.,4.5));
#5929=CARTESIAN_POINT('Origin',(-5.1,1.,1.8));
#5930=CARTESIAN_POINT('',(-5.1,1.,1.8));
#5931=CARTESIAN_POINT('',(-5.1,1.,1.8));
#5932=CARTESIAN_POINT('',(-5.1,1.,1.8));
#5933=CARTESIAN_POINT('Origin',(-5.1,3.2,1.8));
#5934=CARTESIAN_POINT('',(-5.1,3.2,1.8));
#5935=CARTESIAN_POINT('',(-5.1,3.2,1.8));
#5936=CARTESIAN_POINT('',(-5.1,3.2,1.8));
#5937=CARTESIAN_POINT('Origin',(-5.1,3.2,1.));
#5938=CARTESIAN_POINT('',(-5.1,3.2,1.));
#5939=CARTESIAN_POINT('',(-5.1,3.2,1.));
#5940=CARTESIAN_POINT('',(-5.1,3.2,1.));
#5941=CARTESIAN_POINT('Origin',(-5.1,-3.2,1.));
#5942=CARTESIAN_POINT('',(-5.1,-3.2,1.));
#5943=CARTESIAN_POINT('',(-5.1,-3.2,1.));
#5944=CARTESIAN_POINT('',(-5.1,-3.2,1.));
#5945=CARTESIAN_POINT('Origin',(-5.1,-3.2,1.8));
#5946=CARTESIAN_POINT('',(-5.1,-3.2,1.8));
#5947=CARTESIAN_POINT('Origin',(-5.1,0.,3.5));
#5948=CARTESIAN_POINT('',(0.,0.,0.));
#5949=CARTESIAN_POINT('Origin',(-4.5,-2.,7.));
#5950=CARTESIAN_POINT('',(-4.24382623085101,-2.4,7.));
#5951=CARTESIAN_POINT('',(-4.75617376914899,-2.4,7.));
#5952=CARTESIAN_POINT('',(-4.8,-2.4,7.));
#5953=CARTESIAN_POINT('Origin',(-4.5,-2.,7.));
#5954=CARTESIAN_POINT('',(-4.775,-2.,7.));
#5955=CARTESIAN_POINT('Origin',(-4.5,-2.,7.));
#5956=CARTESIAN_POINT('Origin',(-4.5,-2.,7.));
#5957=CARTESIAN_POINT('',(-4.24382623085101,-2.4,7.8));
#5958=CARTESIAN_POINT('',(-4.24382623085101,-2.4,7.));
#5959=CARTESIAN_POINT('',(-4.75617376914899,-2.4,7.8));
#5960=CARTESIAN_POINT('Origin',(-4.5,-2.,7.8));
#5961=CARTESIAN_POINT('',(-4.75617376914899,-2.4,7.));
#5962=CARTESIAN_POINT('Origin',(-4.5,2.,7.));
#5963=CARTESIAN_POINT('',(-4.75617376914899,2.4,7.));
#5964=CARTESIAN_POINT('',(-4.24382623085101,2.4,7.));
#5965=CARTESIAN_POINT('',(-4.2,2.4,7.));
#5966=CARTESIAN_POINT('Origin',(-4.5,2.,7.));
#5967=CARTESIAN_POINT('',(-4.775,2.,7.));
#5968=CARTESIAN_POINT('Origin',(-4.5,2.,7.));
#5969=CARTESIAN_POINT('Origin',(-4.5,2.,7.));
#5970=CARTESIAN_POINT('',(-4.75617376914899,2.4,7.8));
#5971=CARTESIAN_POINT('',(-4.75617376914899,2.4,7.));
#5972=CARTESIAN_POINT('',(-4.24382623085101,2.4,7.8));
#5973=CARTESIAN_POINT('Origin',(-4.5,2.,7.8));
#5974=CARTESIAN_POINT('',(-4.24382623085101,2.4,7.));
#5975=CARTESIAN_POINT('Origin',(-5.1,-2.4,6.));
#5976=CARTESIAN_POINT('',(-5.1,-2.4,7.8));
#5977=CARTESIAN_POINT('',(-5.1,-2.4,7.8));
#5978=CARTESIAN_POINT('',(-5.1,-2.4,6.));
#5979=CARTESIAN_POINT('',(-5.1,-2.4,6.));
#5980=CARTESIAN_POINT('',(-3.9,-2.4,6.));
#5981=CARTESIAN_POINT('',(-5.1,-2.4,6.));
#5982=CARTESIAN_POINT('',(-3.9,-2.4,7.8));
#5983=CARTESIAN_POINT('',(-3.9,-2.4,6.));
#5984=CARTESIAN_POINT('',(-5.1,-2.4,7.8));
#5985=CARTESIAN_POINT('Origin',(-3.9,2.4,6.));
#5986=CARTESIAN_POINT('',(-3.9,2.4,7.8));
#5987=CARTESIAN_POINT('',(-3.9,2.4,7.8));
#5988=CARTESIAN_POINT('',(-3.9,2.4,6.));
#5989=CARTESIAN_POINT('',(-3.9,2.4,6.));
#5990=CARTESIAN_POINT('',(-5.1,2.4,6.));
#5991=CARTESIAN_POINT('',(-3.9,2.4,6.));
#5992=CARTESIAN_POINT('',(-5.1,2.4,7.8));
#5993=CARTESIAN_POINT('',(-5.1,2.4,6.));
#5994=CARTESIAN_POINT('',(-3.9,2.4,7.8));
#5995=CARTESIAN_POINT('Origin',(-4.5,-2.,5.9));
#5996=CARTESIAN_POINT('',(-4.775,-2.,6.));
#5997=CARTESIAN_POINT('Origin',(-4.5,-2.,6.));
#5998=CARTESIAN_POINT('',(-4.775,-2.,5.9));
#5999=CARTESIAN_POINT('Origin',(-4.5,2.,5.9));
#6000=CARTESIAN_POINT('',(-4.775,2.,6.));
#6001=CARTESIAN_POINT('Origin',(-4.5,2.,6.));
#6002=CARTESIAN_POINT('',(-4.775,2.,5.9));
#6003=CARTESIAN_POINT('Origin',(-5.2,0.,6.));
#6004=CARTESIAN_POINT('',(-5.1,1.31,6.));
#6005=CARTESIAN_POINT('',(-5.1,-1.31,6.));
#6006=CARTESIAN_POINT('Origin',(-5.1,0.,6.));
#6007=CARTESIAN_POINT('',(-3.9,1.31,6.));
#6008=CARTESIAN_POINT('',(-5.2,1.31,6.));
#6009=CARTESIAN_POINT('',(-3.9,-1.31,6.));
#6010=CARTESIAN_POINT('Origin',(-3.9,0.,6.));
#6011=CARTESIAN_POINT('',(-5.2,-1.31,6.));
#6012=CARTESIAN_POINT('Origin',(-3.9,-2.4,6.));
#6013=CARTESIAN_POINT('',(-3.9,-2.4,6.));
#6014=CARTESIAN_POINT('',(-3.9,-2.4,7.8));
#6015=CARTESIAN_POINT('',(-3.9,-2.4,6.));
#6016=CARTESIAN_POINT('Origin',(-4.5,0.,6.));
#6017=CARTESIAN_POINT('',(-5.1,2.4,6.));
#6018=CARTESIAN_POINT('Origin',(-5.1,2.4,6.));
#6019=CARTESIAN_POINT('',(-5.1,2.4,6.));
#6020=CARTESIAN_POINT('',(-5.1,2.4,7.8));
#6021=CARTESIAN_POINT('Origin',(-4.5,0.,7.8));
#6022=CARTESIAN_POINT('Origin',(-4.5,0.,6.));
#6023=CARTESIAN_POINT('',(0.,0.,0.));
#6024=CARTESIAN_POINT('Origin',(4.5,-2.,4.9));
#6025=CARTESIAN_POINT('',(4.29,-2.,4.9));
#6026=CARTESIAN_POINT('Origin',(4.5,-2.,4.9));
#6027=CARTESIAN_POINT('',(4.29,-2.,6.));
#6028=CARTESIAN_POINT('',(4.29,-2.,4.9));
#6029=CARTESIAN_POINT('Origin',(4.5,-2.,6.));
#6030=CARTESIAN_POINT('Origin',(4.5,-2.,4.9));
#6031=CARTESIAN_POINT('Origin',(4.5,2.,4.9));
#6032=CARTESIAN_POINT('',(4.29,2.,4.9));
#6033=CARTESIAN_POINT('Origin',(4.5,2.,4.9));
#6034=CARTESIAN_POINT('',(4.29,2.,6.));
#6035=CARTESIAN_POINT('',(4.29,2.,4.9));
#6036=CARTESIAN_POINT('Origin',(4.5,2.,6.));
#6037=CARTESIAN_POINT('Origin',(4.5,2.,4.9));
#6038=CARTESIAN_POINT('Origin',(4.5,-2.6,0.9));
#6039=CARTESIAN_POINT('',(4.225,-2.6,1.));
#6040=CARTESIAN_POINT('Origin',(4.5,-2.6,1.));
#6041=CARTESIAN_POINT('',(4.225,-2.6,1.8));
#6042=CARTESIAN_POINT('',(4.225,-2.6,0.9));
#6043=CARTESIAN_POINT('Origin',(4.5,-2.6,1.8));
#6044=CARTESIAN_POINT('Origin',(4.5,2.6,0.9));
#6045=CARTESIAN_POINT('',(4.225,2.6,1.));
#6046=CARTESIAN_POINT('Origin',(4.5,2.6,1.));
#6047=CARTESIAN_POINT('',(4.225,2.6,1.8));
#6048=CARTESIAN_POINT('',(4.225,2.6,0.9));
#6049=CARTESIAN_POINT('Origin',(4.5,2.6,1.8));
#6050=CARTESIAN_POINT('Origin',(3.8,0.,6.));
#6051=CARTESIAN_POINT('',(5.1,-1.31,6.));
#6052=CARTESIAN_POINT('',(3.9,-1.31,6.));
#6053=CARTESIAN_POINT('',(3.8,-1.31,6.));
#6054=CARTESIAN_POINT('',(5.1,1.31,6.));
#6055=CARTESIAN_POINT('Origin',(5.1,0.,6.));
#6056=CARTESIAN_POINT('',(3.9,1.31,6.));
#6057=CARTESIAN_POINT('',(3.8,1.31,6.));
#6058=CARTESIAN_POINT('Origin',(3.9,0.,6.));
#6059=CARTESIAN_POINT('Origin',(5.1,0.,3.5));
#6060=CARTESIAN_POINT('',(5.1,-2.4,6.));
#6061=CARTESIAN_POINT('',(5.1,2.4,6.));
#6062=CARTESIAN_POINT('',(5.1,-2.4,4.5));
#6063=CARTESIAN_POINT('',(5.1,-2.4,6.));
#6064=CARTESIAN_POINT('',(5.1,-1.,4.5));
#6065=CARTESIAN_POINT('',(5.1,-2.4,4.5));
#6066=CARTESIAN_POINT('',(5.1,-1.,1.8));
#6067=CARTESIAN_POINT('',(5.1,-1.,4.5));
#6068=CARTESIAN_POINT('',(5.1,-3.2,1.8));
#6069=CARTESIAN_POINT('',(5.1,-1.,1.8));
#6070=CARTESIAN_POINT('',(5.1,-3.2,1.));
#6071=CARTESIAN_POINT('',(5.1,-3.2,1.8));
#6072=CARTESIAN_POINT('',(5.1,3.2,1.));
#6073=CARTESIAN_POINT('',(5.1,-3.2,1.));
#6074=CARTESIAN_POINT('',(5.1,3.2,1.8));
#6075=CARTESIAN_POINT('',(5.1,3.2,1.));
#6076=CARTESIAN_POINT('',(5.1,1.,1.8));
#6077=CARTESIAN_POINT('',(5.1,3.2,1.8));
#6078=CARTESIAN_POINT('',(5.1,1.,4.5));
#6079=CARTESIAN_POINT('',(5.1,1.,1.8));
#6080=CARTESIAN_POINT('',(5.1,2.4,4.5));
#6081=CARTESIAN_POINT('',(5.1,1.,4.5));
#6082=CARTESIAN_POINT('',(5.1,2.4,6.));
#6083=CARTESIAN_POINT('',(5.1,2.4,4.5));
#6084=CARTESIAN_POINT('',(5.1,2.4,6.));
#6085=CARTESIAN_POINT('Origin',(3.9,2.4,6.));
#6086=CARTESIAN_POINT('',(3.9,-2.4,6.));
#6087=CARTESIAN_POINT('',(3.9,2.4,6.));
#6088=CARTESIAN_POINT('',(3.9,-2.4,6.));
#6089=CARTESIAN_POINT('Origin',(3.9,2.4,6.));
#6090=CARTESIAN_POINT('',(3.9,2.4,6.));
#6091=CARTESIAN_POINT('',(3.9,2.4,6.));
#6092=CARTESIAN_POINT('',(3.9,2.4,6.));
#6093=CARTESIAN_POINT('Origin',(3.9,-1.,1.8));
#6094=CARTESIAN_POINT('',(3.9,-1.,1.8));
#6095=CARTESIAN_POINT('',(3.9,-3.2,1.8));
#6096=CARTESIAN_POINT('',(3.9,-1.,1.8));
#6097=CARTESIAN_POINT('',(3.9,-3.2,1.8));
#6098=CARTESIAN_POINT('',(3.9,-1.,1.8));
#6099=CARTESIAN_POINT('Origin',(3.9,-1.,4.5));
#6100=CARTESIAN_POINT('',(3.9,-1.,4.5));
#6101=CARTESIAN_POINT('',(3.9,-1.,4.5));
#6102=CARTESIAN_POINT('',(3.9,-1.,4.5));
#6103=CARTESIAN_POINT('Origin',(3.9,-2.4,4.5));
#6104=CARTESIAN_POINT('',(3.9,-2.4,4.5));
#6105=CARTESIAN_POINT('',(3.9,-2.4,4.5));
#6106=CARTESIAN_POINT('',(3.9,-2.4,4.5));
#6107=CARTESIAN_POINT('Origin',(3.9,-2.4,6.));
#6108=CARTESIAN_POINT('',(3.9,-2.4,6.));
#6109=CARTESIAN_POINT('Origin',(3.9,2.4,4.5));
#6110=CARTESIAN_POINT('',(3.9,2.4,4.5));
#6111=CARTESIAN_POINT('',(3.9,2.4,4.5));
#6112=CARTESIAN_POINT('',(3.9,2.4,4.5));
#6113=CARTESIAN_POINT('Origin',(3.9,1.,4.5));
#6114=CARTESIAN_POINT('',(3.9,1.,4.5));
#6115=CARTESIAN_POINT('',(3.9,1.,4.5));
#6116=CARTESIAN_POINT('',(3.9,1.,4.5));
#6117=CARTESIAN_POINT('Origin',(3.9,1.,1.8));
#6118=CARTESIAN_POINT('',(3.9,1.,1.8));
#6119=CARTESIAN_POINT('',(3.9,1.,1.8));
#6120=CARTESIAN_POINT('',(3.9,1.,1.8));
#6121=CARTESIAN_POINT('Origin',(3.9,3.2,1.8));
#6122=CARTESIAN_POINT('',(3.9,3.2,1.8));
#6123=CARTESIAN_POINT('',(3.9,3.2,1.8));
#6124=CARTESIAN_POINT('',(3.9,3.2,1.8));
#6125=CARTESIAN_POINT('Origin',(3.9,3.2,1.));
#6126=CARTESIAN_POINT('',(3.9,3.2,1.));
#6127=CARTESIAN_POINT('',(3.9,3.2,1.));
#6128=CARTESIAN_POINT('',(3.9,3.2,1.));
#6129=CARTESIAN_POINT('Origin',(3.9,-3.2,1.));
#6130=CARTESIAN_POINT('',(3.9,-3.2,1.));
#6131=CARTESIAN_POINT('',(3.9,-3.2,1.));
#6132=CARTESIAN_POINT('',(3.9,-3.2,1.));
#6133=CARTESIAN_POINT('Origin',(3.9,-3.2,1.8));
#6134=CARTESIAN_POINT('',(3.9,-3.2,1.8));
#6135=CARTESIAN_POINT('Origin',(3.9,0.,3.5));
#6136=CARTESIAN_POINT('',(0.,0.,0.));
#6137=CARTESIAN_POINT('Origin',(4.5,-2.,7.));
#6138=CARTESIAN_POINT('',(4.75617376914899,-2.4,7.));
#6139=CARTESIAN_POINT('',(4.24382623085101,-2.4,7.));
#6140=CARTESIAN_POINT('',(4.2,-2.4,7.));
#6141=CARTESIAN_POINT('Origin',(4.5,-2.,7.));
#6142=CARTESIAN_POINT('',(4.225,-2.,7.));
#6143=CARTESIAN_POINT('Origin',(4.5,-2.,7.));
#6144=CARTESIAN_POINT('Origin',(4.5,-2.,7.));
#6145=CARTESIAN_POINT('',(4.75617376914899,-2.4,7.8));
#6146=CARTESIAN_POINT('',(4.75617376914899,-2.4,7.));
#6147=CARTESIAN_POINT('',(4.24382623085101,-2.4,7.8));
#6148=CARTESIAN_POINT('Origin',(4.5,-2.,7.8));
#6149=CARTESIAN_POINT('',(4.24382623085101,-2.4,7.));
#6150=CARTESIAN_POINT('Origin',(4.5,2.,7.));
#6151=CARTESIAN_POINT('',(4.24382623085101,2.4,7.));
#6152=CARTESIAN_POINT('',(4.75617376914899,2.4,7.));
#6153=CARTESIAN_POINT('',(4.8,2.4,7.));
#6154=CARTESIAN_POINT('Origin',(4.5,2.,7.));
#6155=CARTESIAN_POINT('',(4.225,2.,7.));
#6156=CARTESIAN_POINT('Origin',(4.5,2.,7.));
#6157=CARTESIAN_POINT('Origin',(4.5,2.,7.));
#6158=CARTESIAN_POINT('',(4.24382623085101,2.4,7.8));
#6159=CARTESIAN_POINT('',(4.24382623085101,2.4,7.));
#6160=CARTESIAN_POINT('',(4.75617376914899,2.4,7.8));
#6161=CARTESIAN_POINT('Origin',(4.5,2.,7.8));
#6162=CARTESIAN_POINT('',(4.75617376914899,2.4,7.));
#6163=CARTESIAN_POINT('Origin',(3.9,-2.4,6.));
#6164=CARTESIAN_POINT('',(3.9,-2.4,7.8));
#6165=CARTESIAN_POINT('',(3.9,-2.4,7.8));
#6166=CARTESIAN_POINT('',(3.9,-2.4,6.));
#6167=CARTESIAN_POINT('',(3.9,-2.4,6.));
#6168=CARTESIAN_POINT('',(5.1,-2.4,6.));
#6169=CARTESIAN_POINT('',(3.9,-2.4,6.));
#6170=CARTESIAN_POINT('',(5.1,-2.4,7.8));
#6171=CARTESIAN_POINT('',(5.1,-2.4,6.));
#6172=CARTESIAN_POINT('',(3.9,-2.4,7.8));
#6173=CARTESIAN_POINT('Origin',(5.1,2.4,6.));
#6174=CARTESIAN_POINT('',(5.1,2.4,7.8));
#6175=CARTESIAN_POINT('',(5.1,2.4,7.8));
#6176=CARTESIAN_POINT('',(5.1,2.4,6.));
#6177=CARTESIAN_POINT('',(5.1,2.4,6.));
#6178=CARTESIAN_POINT('',(3.9,2.4,6.));
#6179=CARTESIAN_POINT('',(5.1,2.4,6.));
#6180=CARTESIAN_POINT('',(3.9,2.4,7.8));
#6181=CARTESIAN_POINT('',(3.9,2.4,6.));
#6182=CARTESIAN_POINT('',(5.1,2.4,7.8));
#6183=CARTESIAN_POINT('Origin',(4.5,-2.,5.9));
#6184=CARTESIAN_POINT('',(4.225,-2.,6.));
#6185=CARTESIAN_POINT('Origin',(4.5,-2.,6.));
#6186=CARTESIAN_POINT('',(4.225,-2.,5.9));
#6187=CARTESIAN_POINT('Origin',(4.5,2.,5.9));
#6188=CARTESIAN_POINT('',(4.225,2.,6.));
#6189=CARTESIAN_POINT('Origin',(4.5,2.,6.));
#6190=CARTESIAN_POINT('',(4.225,2.,5.9));
#6191=CARTESIAN_POINT('Origin',(3.8,0.,6.));
#6192=CARTESIAN_POINT('',(3.9,1.31,6.));
#6193=CARTESIAN_POINT('',(3.9,-1.31,6.));
#6194=CARTESIAN_POINT('Origin',(3.9,0.,6.));
#6195=CARTESIAN_POINT('',(5.1,1.31,6.));
#6196=CARTESIAN_POINT('',(3.8,1.31,6.));
#6197=CARTESIAN_POINT('',(5.1,-1.31,6.));
#6198=CARTESIAN_POINT('Origin',(5.1,0.,6.));
#6199=CARTESIAN_POINT('',(3.8,-1.31,6.));
#6200=CARTESIAN_POINT('Origin',(5.1,-2.4,6.));
#6201=CARTESIAN_POINT('',(5.1,-2.4,6.));
#6202=CARTESIAN_POINT('',(5.1,-2.4,7.8));
#6203=CARTESIAN_POINT('',(5.1,-2.4,6.));
#6204=CARTESIAN_POINT('Origin',(4.5,0.,6.));
#6205=CARTESIAN_POINT('',(3.9,2.4,6.));
#6206=CARTESIAN_POINT('Origin',(3.9,2.4,6.));
#6207=CARTESIAN_POINT('',(3.9,2.4,6.));
#6208=CARTESIAN_POINT('',(3.9,2.4,7.8));
#6209=CARTESIAN_POINT('Origin',(4.5,0.,7.8));
#6210=CARTESIAN_POINT('Origin',(4.5,0.,6.));
#6211=CARTESIAN_POINT('',(0.,0.,0.));
#6212=CARTESIAN_POINT('Origin',(-6.9,0.,6.));
#6213=CARTESIAN_POINT('',(-6.8,-1.13892152320704E-16,6.93));
#6214=CARTESIAN_POINT('Origin',(-6.8,0.,6.));
#6215=CARTESIAN_POINT('',(-5.45,-1.13892152320704E-16,6.93));
#6216=CARTESIAN_POINT('',(-6.9,-1.13892152320704E-16,6.93));
#6217=CARTESIAN_POINT('Origin',(-5.45,0.,6.));
#6218=CARTESIAN_POINT('Origin',(-5.45,0.,6.));
#6219=CARTESIAN_POINT('',(-5.45,9.67470971326409E-17,6.79));
#6220=CARTESIAN_POINT('Origin',(-5.45,0.,6.));
#6221=CARTESIAN_POINT('Origin',(-6.8,0.,6.));
#6222=CARTESIAN_POINT('',(-2.8,-9.67470971326409E-17,6.79));
#6223=CARTESIAN_POINT('Origin',(-2.8,0.,6.));
#6224=CARTESIAN_POINT('',(-6.8,-9.67470971326409E-17,6.79));
#6225=CARTESIAN_POINT('Origin',(-6.8,0.,6.));
#6226=CARTESIAN_POINT('',(-2.8,-1.59204083889156E-16,7.3));
#6227=CARTESIAN_POINT('Origin',(-2.8,0.,6.));
#6228=CARTESIAN_POINT('',(-6.8,-1.59204083889156E-16,7.3));
#6229=CARTESIAN_POINT('',(-6.8,-1.59204083889156E-16,7.3));
#6230=CARTESIAN_POINT('Origin',(-6.8,0.,6.));
#6231=CARTESIAN_POINT('Origin',(-2.8,0.,6.));
#6232=CARTESIAN_POINT('Origin',(-6.8,0.,6.));
#6233=CARTESIAN_POINT('',(0.,0.,0.));
#6234=CARTESIAN_POINT('Origin',(-0.9,-1.90918830920368,4.09081169079632));
#6235=CARTESIAN_POINT('',(-0.8,-1.90918830920368,4.53081169079632));
#6236=CARTESIAN_POINT('Origin',(-0.8,-1.90918830920368,4.09081169079632));
#6237=CARTESIAN_POINT('',(-0.1,-1.90918830920368,4.53081169079632));
#6238=CARTESIAN_POINT('',(-0.9,-1.90918830920368,4.53081169079632));
#6239=CARTESIAN_POINT('Origin',(-0.1,-1.90918830920368,4.09081169079632));
#6240=CARTESIAN_POINT('Origin',(-0.9,-1.90918830920368,7.90918830920368));
#6241=CARTESIAN_POINT('',(-0.8,-1.90918830920368,8.34918830920368));
#6242=CARTESIAN_POINT('Origin',(-0.8,-1.90918830920368,7.90918830920368));
#6243=CARTESIAN_POINT('',(-0.1,-1.90918830920368,8.34918830920368));
#6244=CARTESIAN_POINT('',(-0.9,-1.90918830920368,8.34918830920368));
#6245=CARTESIAN_POINT('Origin',(-0.1,-1.90918830920368,7.90918830920368));
#6246=CARTESIAN_POINT('Origin',(-0.9,1.90918830920368,7.90918830920368));
#6247=CARTESIAN_POINT('',(-0.8,1.90918830920368,8.34918830920368));
#6248=CARTESIAN_POINT('Origin',(-0.8,1.90918830920368,7.90918830920368));
#6249=CARTESIAN_POINT('',(-0.1,1.90918830920368,8.34918830920368));
#6250=CARTESIAN_POINT('',(-0.9,1.90918830920368,8.34918830920368));
#6251=CARTESIAN_POINT('Origin',(-0.1,1.90918830920368,7.90918830920368));
#6252=CARTESIAN_POINT('Origin',(-0.9,1.90918830920368,4.09081169079632));
#6253=CARTESIAN_POINT('',(-0.8,1.90918830920368,4.53081169079632));
#6254=CARTESIAN_POINT('Origin',(-0.8,1.90918830920368,4.09081169079632));
#6255=CARTESIAN_POINT('',(-0.1,1.90918830920368,4.53081169079632));
#6256=CARTESIAN_POINT('',(-0.9,1.90918830920368,4.53081169079632));
#6257=CARTESIAN_POINT('Origin',(-0.1,1.90918830920368,4.09081169079632));
#6258=CARTESIAN_POINT('Origin',(-0.8,0.,6.));
#6259=CARTESIAN_POINT('',(-0.8,-4.28626379701574E-16,9.5));
#6260=CARTESIAN_POINT('Origin',(-0.8,0.,6.));
#6261=CARTESIAN_POINT('',(-0.8,1.83697019872103E-16,7.5));
#6262=CARTESIAN_POINT('Origin',(-0.8,0.,6.));
#6263=CARTESIAN_POINT('Origin',(-0.8,0.,6.));
#6264=CARTESIAN_POINT('',(-0.1,-4.28626379701574E-16,9.5));
#6265=CARTESIAN_POINT('Origin',(-0.1,0.,6.));
#6266=CARTESIAN_POINT('',(-0.8,-4.28626379701574E-16,9.5));
#6267=CARTESIAN_POINT('Origin',(-2.8,0.,6.));
#6268=CARTESIAN_POINT('',(-0.1,-9.67470971326409E-17,6.79));
#6269=CARTESIAN_POINT('Origin',(-0.1,0.,6.));
#6270=CARTESIAN_POINT('',(-2.8,-9.67470971326409E-17,6.79));
#6271=CARTESIAN_POINT('',(-2.8,-9.67470971326409E-17,6.79));
#6272=CARTESIAN_POINT('Origin',(-2.8,0.,6.));
#6273=CARTESIAN_POINT('Origin',(-2.8,0.,6.));
#6274=CARTESIAN_POINT('',(-2.8,-1.83697019872103E-16,7.5));
#6275=CARTESIAN_POINT('',(-2.8,-1.83697019872103E-16,7.5));
#6276=CARTESIAN_POINT('Origin',(-2.8,0.,6.));
#6277=CARTESIAN_POINT('Origin',(-0.1,0.,6.));
#6278=CARTESIAN_POINT('Origin',(-2.8,0.,6.));
#6279=CARTESIAN_POINT('',(0.,0.,0.));
#6280=CARTESIAN_POINT('Origin',(5.45,0.,6.));
#6281=CARTESIAN_POINT('',(5.45,-1.13892152320704E-16,6.93));
#6282=CARTESIAN_POINT('Origin',(5.45,0.,6.));
#6283=CARTESIAN_POINT('',(6.8,1.13892152320704E-16,6.93));
#6284=CARTESIAN_POINT('',(5.45,-1.13892152320704E-16,6.93));
#6285=CARTESIAN_POINT('Origin',(6.8,0.,6.));
#6286=CARTESIAN_POINT('Origin',(5.45,0.,6.));
#6287=CARTESIAN_POINT('',(5.45,-9.67470971326409E-17,6.79));
#6288=CARTESIAN_POINT('Origin',(5.45,0.,6.));
#6289=CARTESIAN_POINT('Origin',(2.8,0.,6.));
#6290=CARTESIAN_POINT('',(2.8,-9.67470971326409E-17,6.79));
#6291=CARTESIAN_POINT('',(2.8,-9.67470971326409E-17,6.79));
#6292=CARTESIAN_POINT('Origin',(2.8,0.,6.));
#6293=CARTESIAN_POINT('Origin',(2.8,0.,6.));
#6294=CARTESIAN_POINT('',(6.8,-1.59204083889156E-16,7.3));
#6295=CARTESIAN_POINT('Origin',(6.8,0.,6.));
#6296=CARTESIAN_POINT('',(2.8,-1.59204083889156E-16,7.3));
#6297=CARTESIAN_POINT('',(2.8,-1.59204083889156E-16,7.3));
#6298=CARTESIAN_POINT('Origin',(2.8,0.,6.));
#6299=CARTESIAN_POINT('Origin',(6.8,0.,6.));
#6300=CARTESIAN_POINT('Origin',(2.8,0.,6.));
#6301=CARTESIAN_POINT('',(0.,0.,0.));
#6302=CARTESIAN_POINT('Origin',(0.,-1.90918830920368,4.09081169079632));
#6303=CARTESIAN_POINT('',(0.1,-1.90918830920368,4.53081169079632));
#6304=CARTESIAN_POINT('Origin',(0.1,-1.90918830920368,4.09081169079632));
#6305=CARTESIAN_POINT('',(0.8,-1.90918830920368,4.53081169079632));
#6306=CARTESIAN_POINT('',(0.,-1.90918830920368,4.53081169079632));
#6307=CARTESIAN_POINT('Origin',(0.8,-1.90918830920368,4.09081169079632));
#6308=CARTESIAN_POINT('Origin',(0.,-1.90918830920368,7.90918830920368));
#6309=CARTESIAN_POINT('',(0.1,-1.90918830920368,8.34918830920368));
#6310=CARTESIAN_POINT('Origin',(0.1,-1.90918830920368,7.90918830920368));
#6311=CARTESIAN_POINT('',(0.8,-1.90918830920368,8.34918830920368));
#6312=CARTESIAN_POINT('',(0.,-1.90918830920368,8.34918830920368));
#6313=CARTESIAN_POINT('Origin',(0.8,-1.90918830920368,7.90918830920368));
#6314=CARTESIAN_POINT('Origin',(0.,1.90918830920368,7.90918830920368));
#6315=CARTESIAN_POINT('',(0.1,1.90918830920368,8.34918830920368));
#6316=CARTESIAN_POINT('Origin',(0.1,1.90918830920368,7.90918830920368));
#6317=CARTESIAN_POINT('',(0.8,1.90918830920368,8.34918830920368));
#6318=CARTESIAN_POINT('',(0.,1.90918830920368,8.34918830920368));
#6319=CARTESIAN_POINT('Origin',(0.8,1.90918830920368,7.90918830920368));
#6320=CARTESIAN_POINT('Origin',(0.,1.90918830920368,4.09081169079632));
#6321=CARTESIAN_POINT('',(0.1,1.90918830920368,4.53081169079632));
#6322=CARTESIAN_POINT('Origin',(0.1,1.90918830920368,4.09081169079632));
#6323=CARTESIAN_POINT('',(0.8,1.90918830920368,4.53081169079632));
#6324=CARTESIAN_POINT('',(0.,1.90918830920368,4.53081169079632));
#6325=CARTESIAN_POINT('Origin',(0.8,1.90918830920368,4.09081169079632));
#6326=CARTESIAN_POINT('Origin',(0.8,0.,6.));
#6327=CARTESIAN_POINT('',(0.8,-4.28626379701574E-16,9.5));
#6328=CARTESIAN_POINT('Origin',(0.8,0.,6.));
#6329=CARTESIAN_POINT('',(0.8,-1.83697019872103E-16,7.5));
#6330=CARTESIAN_POINT('Origin',(0.8,0.,6.));
#6331=CARTESIAN_POINT('Origin',(0.1,0.,6.));
#6332=CARTESIAN_POINT('',(0.1,-4.28626379701574E-16,9.5));
#6333=CARTESIAN_POINT('',(0.1,-4.28626379701574E-16,9.5));
#6334=CARTESIAN_POINT('Origin',(0.1,0.,6.));
#6335=CARTESIAN_POINT('Origin',(0.1,0.,6.));
#6336=CARTESIAN_POINT('',(2.8,-9.67470971326409E-17,6.79));
#6337=CARTESIAN_POINT('Origin',(2.8,0.,6.));
#6338=CARTESIAN_POINT('',(0.1,-9.67470971326409E-17,6.79));
#6339=CARTESIAN_POINT('',(0.1,-9.67470971326409E-17,6.79));
#6340=CARTESIAN_POINT('Origin',(0.1,0.,6.));
#6341=CARTESIAN_POINT('Origin',(0.1,0.,6.));
#6342=CARTESIAN_POINT('',(2.8,-1.83697019872103E-16,7.5));
#6343=CARTESIAN_POINT('Origin',(2.8,0.,6.));
#6344=CARTESIAN_POINT('',(0.1,-1.83697019872103E-16,7.5));
#6345=CARTESIAN_POINT('Origin',(2.8,0.,6.));
#6346=CARTESIAN_POINT('Origin',(0.1,0.,6.));
#6347=CARTESIAN_POINT('',(0.,0.,0.));
#6348=CARTESIAN_POINT('Origin',(-0.1,0.,6.));
#6349=CARTESIAN_POINT('',(0.1,-9.67470971326409E-17,6.79));
#6350=CARTESIAN_POINT('Origin',(0.1,0.,6.));
#6351=CARTESIAN_POINT('',(-0.1,-9.67470971326409E-17,6.79));
#6352=CARTESIAN_POINT('',(-0.1,-9.67470971326409E-17,6.79));
#6353=CARTESIAN_POINT('Origin',(-0.1,0.,6.));
#6354=CARTESIAN_POINT('Origin',(-0.1,0.,6.));
#6355=CARTESIAN_POINT('',(0.1,-2.69422295812418E-16,8.2));
#6356=CARTESIAN_POINT('Origin',(0.1,0.,6.));
#6357=CARTESIAN_POINT('',(-0.1,-2.69422295812418E-16,8.2));
#6358=CARTESIAN_POINT('',(-0.1,-2.69422295812418E-16,8.2));
#6359=CARTESIAN_POINT('Origin',(-0.1,0.,6.));
#6360=CARTESIAN_POINT('Origin',(0.1,0.,6.));
#6361=CARTESIAN_POINT('Origin',(-0.1,0.,6.));
#6362=CARTESIAN_POINT('',(0.,0.,0.));
#6363=CARTESIAN_POINT('Origin',(0.115470053837925,-0.5,-0.2));
#6364=CARTESIAN_POINT('',(0.23094010767585,-0.5,0.));
#6365=CARTESIAN_POINT('',(0.115470053837925,-0.5,-0.2));
#6366=CARTESIAN_POINT('',(0.23094010767585,-0.5,0.));
#6367=CARTESIAN_POINT('',(0.115470053837925,-0.8,-0.2));
#6368=CARTESIAN_POINT('',(0.115470053837925,-0.5,-0.2));
#6369=CARTESIAN_POINT('',(0.23094010767585,-0.8,0.));
#6370=CARTESIAN_POINT('',(0.23094010767585,-0.8,0.));
#6371=CARTESIAN_POINT('',(0.23094010767585,-0.5,0.));
#6372=CARTESIAN_POINT('Origin',(-0.115470053837925,-0.5,-0.2));
#6373=CARTESIAN_POINT('',(-0.115470053837925,-0.5,-0.2));
#6374=CARTESIAN_POINT('',(0.115470053837925,-0.5,-0.2));
#6375=CARTESIAN_POINT('',(-0.115470053837925,-0.8,-0.2));
#6376=CARTESIAN_POINT('',(-0.115470053837925,-0.5,-0.2));
#6377=CARTESIAN_POINT('',(0.115470053837925,-0.8,-0.2));
#6378=CARTESIAN_POINT('Origin',(-0.23094010767585,-0.5,-2.77555756156289E-17));
#6379=CARTESIAN_POINT('',(-0.23094010767585,-0.5,-2.82820063659975E-17));
#6380=CARTESIAN_POINT('',(-0.115470053837925,-0.5,-0.2));
#6381=CARTESIAN_POINT('',(-0.23094010767585,-0.8,-2.77555756156289E-17));
#6382=CARTESIAN_POINT('',(-0.23094010767585,-0.5,-2.82820063659975E-17));
#6383=CARTESIAN_POINT('',(-0.115470053837925,-0.8,-0.2));
#6384=CARTESIAN_POINT('Origin',(-0.115470053837925,-0.5,0.2));
#6385=CARTESIAN_POINT('',(-0.115470053837925,-0.5,0.2));
#6386=CARTESIAN_POINT('',(-0.23094010767585,-0.5,-2.82820063659975E-17));
#6387=CARTESIAN_POINT('',(-0.115470053837925,-0.8,0.2));
#6388=CARTESIAN_POINT('',(-0.115470053837925,-0.5,0.2));
#6389=CARTESIAN_POINT('',(-0.23094010767585,-0.8,-2.82820063659975E-17));
#6390=CARTESIAN_POINT('Origin',(0.115470053837925,-0.5,0.2));
#6391=CARTESIAN_POINT('',(0.115470053837925,-0.5,0.2));
#6392=CARTESIAN_POINT('',(-0.115470053837925,-0.5,0.2));
#6393=CARTESIAN_POINT('',(0.115470053837925,-0.8,0.2));
#6394=CARTESIAN_POINT('',(0.115470053837925,-0.5,0.2));
#6395=CARTESIAN_POINT('',(-0.115470053837925,-0.8,0.2));
#6396=CARTESIAN_POINT('Origin',(0.23094010767585,-0.5,0.));
#6397=CARTESIAN_POINT('',(0.115470053837925,-0.5,0.2));
#6398=CARTESIAN_POINT('',(0.115470053837925,-0.8,0.2));
#6399=CARTESIAN_POINT('Origin',(0.,-0.5,0.));
#6400=CARTESIAN_POINT('Origin',(0.,-0.8,0.));
#6401=CARTESIAN_POINT('Origin',(0.,-1.4,0.));
#6402=CARTESIAN_POINT('',(-0.24505,-1.4,3.00099698131059E-17));
#6403=CARTESIAN_POINT('Origin',(0.,-1.4,0.));
#6404=CARTESIAN_POINT('Origin',(0.375,0.5,0.));
#6405=CARTESIAN_POINT('',(-0.375,0.5,-4.59242549680257E-17));
#6406=CARTESIAN_POINT('Origin',(0.,0.5,0.));
#6407=CARTESIAN_POINT('Origin',(0.,0.475,0.));
#6408=CARTESIAN_POINT('',(-0.425,0.45,-5.20474889637625E-17));
#6409=CARTESIAN_POINT('Origin',(0.,0.45,0.));
#6410=CARTESIAN_POINT('',(-0.4,0.475,-4.89858719658941E-17));
#6411=CARTESIAN_POINT('Origin',(0.,0.24,0.));
#6412=CARTESIAN_POINT('',(-0.425,0.0299999999999998,-5.20474889637625E-17));
#6413=CARTESIAN_POINT('Origin',(0.,0.0299999999999998,0.));
#6414=CARTESIAN_POINT('',(-0.425,0.24,-5.20474889637625E-17));
#6415=CARTESIAN_POINT('Origin',(0.,0.0150000000000001,0.));
#6416=CARTESIAN_POINT('',(-0.395,4.85722573273506E-17,-4.83735485663204E-17));
#6417=CARTESIAN_POINT('Origin',(0.,0.,0.));
#6418=CARTESIAN_POINT('',(-0.41,0.0150000000000001,-5.02105187650415E-17));
#6419=CARTESIAN_POINT('Origin',(0.27,0.,0.));
#6420=CARTESIAN_POINT('',(-0.27,0.,-3.30654635769785E-17));
#6421=CARTESIAN_POINT('Origin',(0.,0.,0.));
#6422=CARTESIAN_POINT('Origin',(0.,-0.02,0.));
#6423=CARTESIAN_POINT('',(-0.24505,-0.0498999999999999,3.00099698131059E-17));
#6424=CARTESIAN_POINT('Origin',(0.,-0.0498999999999999,0.));
#6425=CARTESIAN_POINT('',(-0.26,-0.02,-3.18408167778312E-17));
#6426=CARTESIAN_POINT('Origin',(0.,-0.995,0.));
#6427=CARTESIAN_POINT('',(-0.24505,-0.995,-3.00099698131059E-17));
#6428=CARTESIAN_POINT('',(0.,0.,0.));
#6429=CARTESIAN_POINT('Origin',(0.375,0.5,0.));
#6430=CARTESIAN_POINT('',(-0.375,0.5,-4.59242549680257E-17));
#6431=CARTESIAN_POINT('Origin',(0.,0.5,0.));
#6432=CARTESIAN_POINT('Origin',(0.,0.475,0.));
#6433=CARTESIAN_POINT('',(-0.425,0.45,-5.20474889637625E-17));
#6434=CARTESIAN_POINT('Origin',(0.,0.45,0.));
#6435=CARTESIAN_POINT('',(-0.4,0.475,-4.89858719658941E-17));
#6436=CARTESIAN_POINT('Origin',(0.,0.24,0.));
#6437=CARTESIAN_POINT('',(-0.425,0.0299999999999998,-5.20474889637625E-17));
#6438=CARTESIAN_POINT('Origin',(0.,0.0299999999999998,0.));
#6439=CARTESIAN_POINT('',(-0.425,0.24,-5.20474889637625E-17));
#6440=CARTESIAN_POINT('Origin',(0.,0.0150000000000001,0.));
#6441=CARTESIAN_POINT('',(-0.395,4.85722573273506E-17,-4.83735485663204E-17));
#6442=CARTESIAN_POINT('Origin',(0.,0.,0.));
#6443=CARTESIAN_POINT('',(-0.41,0.0150000000000001,-5.02105187650415E-17));
#6444=CARTESIAN_POINT('Origin',(0.27,0.,0.));
#6445=CARTESIAN_POINT('',(-0.27,0.,-3.30654635769785E-17));
#6446=CARTESIAN_POINT('Origin',(0.,0.,0.));
#6447=CARTESIAN_POINT('Origin',(0.,-0.02,0.));
#6448=CARTESIAN_POINT('',(-0.24505,-0.0498999999999999,3.00099698131059E-17));
#6449=CARTESIAN_POINT('Origin',(0.,-0.0498999999999999,0.));
#6450=CARTESIAN_POINT('',(-0.26,-0.02,-3.18408167778312E-17));
#6451=CARTESIAN_POINT('Origin',(0.,-0.995,0.));
#6452=CARTESIAN_POINT('',(-0.24505,-1.95495,3.00099698131059E-17));
#6453=CARTESIAN_POINT('Origin',(0.,-1.95495,0.));
#6454=CARTESIAN_POINT('',(-0.24505,-0.995,-3.00099698131059E-17));
#6455=CARTESIAN_POINT('Origin',(0.,-1.975,0.));
#6456=CARTESIAN_POINT('',(-0.2,-2.,-2.44929359829471E-17));
#6457=CARTESIAN_POINT('Origin',(0.,-2.,0.));
#6458=CARTESIAN_POINT('',(-0.225,-1.975,-2.75545529808154E-17));
#6459=CARTESIAN_POINT('Origin',(0.,-2.,0.));
#6460=CARTESIAN_POINT('Origin',(0.115470053837925,-0.5,-0.2));
#6461=CARTESIAN_POINT('',(0.23094010767585,-0.5,0.));
#6462=CARTESIAN_POINT('',(0.115470053837925,-0.5,-0.2));
#6463=CARTESIAN_POINT('',(0.23094010767585,-0.5,0.));
#6464=CARTESIAN_POINT('',(0.115470053837925,-0.8,-0.2));
#6465=CARTESIAN_POINT('',(0.115470053837925,-0.5,-0.2));
#6466=CARTESIAN_POINT('',(0.23094010767585,-0.8,0.));
#6467=CARTESIAN_POINT('',(0.23094010767585,-0.8,0.));
#6468=CARTESIAN_POINT('',(0.23094010767585,-0.5,0.));
#6469=CARTESIAN_POINT('Origin',(-0.115470053837925,-0.5,-0.2));
#6470=CARTESIAN_POINT('',(-0.115470053837925,-0.5,-0.2));
#6471=CARTESIAN_POINT('',(0.115470053837925,-0.5,-0.2));
#6472=CARTESIAN_POINT('',(-0.115470053837925,-0.8,-0.2));
#6473=CARTESIAN_POINT('',(-0.115470053837925,-0.5,-0.2));
#6474=CARTESIAN_POINT('',(0.115470053837925,-0.8,-0.2));
#6475=CARTESIAN_POINT('Origin',(-0.23094010767585,-0.5,-2.77555756156289E-17));
#6476=CARTESIAN_POINT('',(-0.23094010767585,-0.5,-2.82820063659975E-17));
#6477=CARTESIAN_POINT('',(-0.115470053837925,-0.5,-0.2));
#6478=CARTESIAN_POINT('',(-0.23094010767585,-0.8,-2.77555756156289E-17));
#6479=CARTESIAN_POINT('',(-0.23094010767585,-0.5,-2.82820063659975E-17));
#6480=CARTESIAN_POINT('',(-0.115470053837925,-0.8,-0.2));
#6481=CARTESIAN_POINT('Origin',(-0.115470053837925,-0.5,0.2));
#6482=CARTESIAN_POINT('',(-0.115470053837925,-0.5,0.2));
#6483=CARTESIAN_POINT('',(-0.23094010767585,-0.5,-2.82820063659975E-17));
#6484=CARTESIAN_POINT('',(-0.115470053837925,-0.8,0.2));
#6485=CARTESIAN_POINT('',(-0.115470053837925,-0.5,0.2));
#6486=CARTESIAN_POINT('',(-0.23094010767585,-0.8,-2.82820063659975E-17));
#6487=CARTESIAN_POINT('Origin',(0.115470053837925,-0.5,0.2));
#6488=CARTESIAN_POINT('',(0.115470053837925,-0.5,0.2));
#6489=CARTESIAN_POINT('',(-0.115470053837925,-0.5,0.2));
#6490=CARTESIAN_POINT('',(0.115470053837925,-0.8,0.2));
#6491=CARTESIAN_POINT('',(0.115470053837925,-0.5,0.2));
#6492=CARTESIAN_POINT('',(-0.115470053837925,-0.8,0.2));
#6493=CARTESIAN_POINT('Origin',(0.23094010767585,-0.5,0.));
#6494=CARTESIAN_POINT('',(0.115470053837925,-0.5,0.2));
#6495=CARTESIAN_POINT('',(0.115470053837925,-0.8,0.2));
#6496=CARTESIAN_POINT('Origin',(0.,-0.5,0.));
#6497=CARTESIAN_POINT('Origin',(0.,-0.8,0.));
#6498=CARTESIAN_POINT('',(0.,0.,0.));
#6499=CARTESIAN_POINT('Origin',(0.,0.,0.));
#6500=CARTESIAN_POINT('',(0.276530287672074,0.276530287672074,0.740020945649513));
#6501=CARTESIAN_POINT('',(0.276530287672074,0.276530287672074,-0.740020945649513));
#6502=CARTESIAN_POINT('Origin',(0.,0.,0.));
#6503=CARTESIAN_POINT('',(-0.79,0.276530287672074,9.67470971326409E-17));
#6504=CARTESIAN_POINT('Origin',(0.,0.276530287672074,0.));
#6505=CARTESIAN_POINT('',(-0.79,1.45,-9.67470971326409E-17));
#6506=CARTESIAN_POINT('',(-0.79,0.,9.67470971326409E-17));
#6507=CARTESIAN_POINT('Origin',(0.,1.45,0.));
#6508=CARTESIAN_POINT('Origin',(0.,0.276530287672074,0.));
#6509=CARTESIAN_POINT('Origin',(0.,0.,0.));
#6510=CARTESIAN_POINT('',(-5.12514685443167E-17,-6.27649469043988E-33,-0.837));
#6511=CARTESIAN_POINT('',(-5.12514685443167E-17,-6.27649469043988E-33,0.837));
#6512=CARTESIAN_POINT('Origin',(0.,0.,0.));
#6513=CARTESIAN_POINT('',(0.276530287672074,-9.67470971326409E-17,0.79));
#6514=CARTESIAN_POINT('Origin',(0.276530287672074,0.,0.));
#6515=CARTESIAN_POINT('Origin',(0.276530287672074,0.,0.));
#6516=CARTESIAN_POINT('Origin',(0.,0.,0.));
#6517=CARTESIAN_POINT('',(1.45,9.67470971326409E-17,0.79));
#6518=CARTESIAN_POINT('',(0.,-9.67470971326409E-17,0.79));
#6519=CARTESIAN_POINT('Origin',(1.45,0.,0.));
#6520=CARTESIAN_POINT('Origin',(0.,1.45,0.));
#6521=CARTESIAN_POINT('',(-0.93,1.45,-1.13892152320704E-16));
#6522=CARTESIAN_POINT('Origin',(0.,1.45,0.));
#6523=CARTESIAN_POINT('Origin',(0.,2.175,0.));
#6524=CARTESIAN_POINT('',(-0.93,2.8,-1.13892152320704E-16));
#6525=CARTESIAN_POINT('Origin',(0.,2.8,0.));
#6526=CARTESIAN_POINT('',(-0.93,2.175,-1.13892152320704E-16));
#6527=CARTESIAN_POINT('Origin',(2.175,0.,0.));
#6528=CARTESIAN_POINT('',(1.45,-0.93,-1.13892152320704E-16));
#6529=CARTESIAN_POINT('Origin',(1.45,0.,0.));
#6530=CARTESIAN_POINT('',(2.8,-0.93,1.13892152320704E-16));
#6531=CARTESIAN_POINT('',(2.175,-0.93,-1.13892152320704E-16));
#6532=CARTESIAN_POINT('Origin',(2.8,0.,0.));
#6533=CARTESIAN_POINT('Origin',(1.45,0.93,0.));
#6534=CARTESIAN_POINT('Origin',(0.,0.,0.));
#6535=CARTESIAN_POINT('',(0.,0.,1.2));
#6536=CARTESIAN_POINT('',(-1.2,1.11022302462516E-16,-1.46957615897682E-16));
#6537=CARTESIAN_POINT('Origin',(0.,0.,0.));
#6538=CARTESIAN_POINT('',(0.,0.,-1.2));
#6539=CARTESIAN_POINT('Origin',(0.,0.,0.));
#6540=CARTESIAN_POINT('',(1.11022302462516E-16,-1.2,-1.46957615897682E-16));
#6541=CARTESIAN_POINT('Origin',(0.,0.,0.));
#6542=CARTESIAN_POINT('Origin',(0.,0.,0.));
#6543=CARTESIAN_POINT('Origin',(0.,0.9,0.));
#6544=CARTESIAN_POINT('Origin',(0.,0.,0.));
#6545=CARTESIAN_POINT('',(-1.2,1.8,-1.46957615897682E-16));
#6546=CARTESIAN_POINT('',(-1.2,0.9,-1.46957615897682E-16));
#6547=CARTESIAN_POINT('Origin',(0.,1.8,0.));
#6548=CARTESIAN_POINT('Origin',(1.45,2.8,0.));
#6549=CARTESIAN_POINT('',(-1.45,2.8,-1.77573785876366E-16));
#6550=CARTESIAN_POINT('Origin',(0.,2.8,0.));
#6551=CARTESIAN_POINT('Origin',(0.,2.3,0.));
#6552=CARTESIAN_POINT('',(-1.45,1.8,-1.77573785876366E-16));
#6553=CARTESIAN_POINT('Origin',(0.,1.8,0.));
#6554=CARTESIAN_POINT('',(-1.45,2.3,-1.77573785876366E-16));
#6555=CARTESIAN_POINT('Origin',(1.2,1.8,0.));
#6556=CARTESIAN_POINT('Origin',(1.8,1.45,0.));
#6557=CARTESIAN_POINT('',(1.8,-1.45,-1.77573785876366E-16));
#6558=CARTESIAN_POINT('Origin',(1.8,0.,0.));
#6559=CARTESIAN_POINT('',(1.8,-1.2,-1.46957615897682E-16));
#6560=CARTESIAN_POINT('Origin',(1.8,0.,0.));
#6561=CARTESIAN_POINT('Origin',(2.3,0.,0.));
#6562=CARTESIAN_POINT('',(2.8,-1.45,-1.77573785876366E-16));
#6563=CARTESIAN_POINT('Origin',(2.8,0.,0.));
#6564=CARTESIAN_POINT('',(2.3,-1.45,-1.77573785876366E-16));
#6565=CARTESIAN_POINT('Origin',(2.8,0.,0.));
#6566=CARTESIAN_POINT('Origin',(0.9,0.,0.));
#6567=CARTESIAN_POINT('',(0.9,-1.2,-1.46957615897682E-16));
#6568=CARTESIAN_POINT('',(0.,0.,0.));
#6569=CARTESIAN_POINT('Origin',(0.,-0.6,0.));
#6570=CARTESIAN_POINT('',(1.55884572681199,-0.6,0.));
#6571=CARTESIAN_POINT('',(0.779422863405995,-0.6,1.35));
#6572=CARTESIAN_POINT('',(0.779422863405995,-0.6,1.35));
#6573=CARTESIAN_POINT('',(-0.779422863405996,-0.6,1.35));
#6574=CARTESIAN_POINT('',(-0.779422863405996,-0.6,1.35));
#6575=CARTESIAN_POINT('',(-1.55884572681199,-0.6,-1.90903542970483E-16));
#6576=CARTESIAN_POINT('',(-1.55884572681199,-0.6,-1.90903542970483E-16));
#6577=CARTESIAN_POINT('',(-0.779422863405995,-0.6,-1.35));
#6578=CARTESIAN_POINT('',(-0.779422863405995,-0.6,-1.35));
#6579=CARTESIAN_POINT('',(0.779422863405995,-0.6,-1.35));
#6580=CARTESIAN_POINT('',(0.779422863405995,-0.6,-1.35));
#6581=CARTESIAN_POINT('',(1.55884572681199,-0.6,0.));
#6582=CARTESIAN_POINT('',(-1.065,-0.6,-1.30424884109193E-16));
#6583=CARTESIAN_POINT('Origin',(0.,-0.6,0.));
#6584=CARTESIAN_POINT('Origin',(0.,0.6,0.));
#6585=CARTESIAN_POINT('',(0.779422863405995,0.6,1.35));
#6586=CARTESIAN_POINT('',(1.55884572681199,0.6,0.));
#6587=CARTESIAN_POINT('',(0.779422863405995,0.6,1.35));
#6588=CARTESIAN_POINT('',(0.779422863405995,0.6,-1.35));
#6589=CARTESIAN_POINT('',(1.55884572681199,0.6,0.));
#6590=CARTESIAN_POINT('',(-0.779422863405995,0.6,-1.35));
#6591=CARTESIAN_POINT('',(0.779422863405995,0.6,-1.35));
#6592=CARTESIAN_POINT('',(-1.55884572681199,0.6,-1.90903542970483E-16));
#6593=CARTESIAN_POINT('',(-0.779422863405995,0.6,-1.35));
#6594=CARTESIAN_POINT('',(-0.779422863405996,0.6,1.35));
#6595=CARTESIAN_POINT('',(-1.55884572681199,0.6,-1.90903542970483E-16));
#6596=CARTESIAN_POINT('',(-0.779422863405996,0.6,1.35));
#6597=CARTESIAN_POINT('',(-1.065,0.6,1.30424884109193E-16));
#6598=CARTESIAN_POINT('Origin',(0.,0.6,0.));
#6599=CARTESIAN_POINT('Origin',(-0.779422863405996,0.,1.35));
#6600=CARTESIAN_POINT('',(0.779422863405995,0.,1.35));
#6601=CARTESIAN_POINT('',(-0.779422863405996,0.,1.35));
#6602=CARTESIAN_POINT('Origin',(-1.55884572681199,0.,-1.90903542970483E-16));
#6603=CARTESIAN_POINT('',(-1.55884572681199,0.,-1.90903542970483E-16));
#6604=CARTESIAN_POINT('Origin',(-0.779422863405995,0.,-1.35));
#6605=CARTESIAN_POINT('',(-0.779422863405995,0.,-1.35));
#6606=CARTESIAN_POINT('Origin',(0.779422863405995,0.,-1.35));
#6607=CARTESIAN_POINT('',(0.779422863405995,0.,-1.35));
#6608=CARTESIAN_POINT('Origin',(1.55884572681199,0.,0.));
#6609=CARTESIAN_POINT('',(1.55884572681199,0.,0.));
#6610=CARTESIAN_POINT('Origin',(0.779422863405995,0.,1.35));
#6611=CARTESIAN_POINT('Origin',(0.,0.,0.));
#6612=CARTESIAN_POINT('',(-1.065,2.47,-1.30424884109193E-16));
#6613=CARTESIAN_POINT('',(-1.065,0.,-1.30424884109193E-16));
#6614=CARTESIAN_POINT('Origin',(0.,2.47,0.));
#6615=CARTESIAN_POINT('Origin',(0.985,2.55,0.));
#6616=CARTESIAN_POINT('',(-0.985,2.55,-1.20627709716014E-16));
#6617=CARTESIAN_POINT('Origin',(0.,2.55,0.));
#6618=CARTESIAN_POINT('',(-0.79,2.55,-9.67470971326409E-17));
#6619=CARTESIAN_POINT('Origin',(0.,2.55,0.));
#6620=CARTESIAN_POINT('Origin',(0.,2.51,0.));
#6621=CARTESIAN_POINT('',(-1.025,2.51,-1.25526296912604E-16));
#6622=CARTESIAN_POINT('Origin',(0.,0.,0.));
#6623=CARTESIAN_POINT('',(-1.065,-2.47,-1.30424884109193E-16));
#6624=CARTESIAN_POINT('Origin',(0.,-2.47,0.));
#6625=CARTESIAN_POINT('',(-1.065,0.,-1.30424884109193E-16));
#6626=CARTESIAN_POINT('Origin',(0.,-2.51,0.));
#6627=CARTESIAN_POINT('',(-0.985,-2.55,-1.20627709716014E-16));
#6628=CARTESIAN_POINT('Origin',(0.,-2.55,0.));
#6629=CARTESIAN_POINT('',(-1.025,-2.51,-1.25526296912604E-16));
#6630=CARTESIAN_POINT('Origin',(0.79,-2.55,0.));
#6631=CARTESIAN_POINT('',(-0.79,-2.55,-9.67470971326409E-17));
#6632=CARTESIAN_POINT('Origin',(0.,-2.55,0.));
#6633=CARTESIAN_POINT('Origin',(0.,0.,0.));
#6634=CARTESIAN_POINT('',(-0.79,0.,-9.67470971326409E-17));
#6635=CARTESIAN_POINT('',(0.,0.,0.));
#6636=CARTESIAN_POINT('Origin',(0.6,0.8,0.));
#6637=CARTESIAN_POINT('',(-0.6,0.8,-7.34788079488412E-17));
#6638=CARTESIAN_POINT('Origin',(0.,0.8,0.));
#6639=CARTESIAN_POINT('Origin',(0.,0.775,0.));
#6640=CARTESIAN_POINT('',(-0.65,0.75,-7.9602041944578E-17));
#6641=CARTESIAN_POINT('Origin',(0.,0.75,0.));
#6642=CARTESIAN_POINT('',(-0.625,0.775,-7.65404249467096E-17));
#6643=CARTESIAN_POINT('Origin',(0.,0.39,0.));
#6644=CARTESIAN_POINT('',(-0.65,0.0299999999999998,-7.9602041944578E-17));
#6645=CARTESIAN_POINT('Origin',(0.,0.0299999999999998,0.));
#6646=CARTESIAN_POINT('',(-0.65,0.39,-7.9602041944578E-17));
#6647=CARTESIAN_POINT('Origin',(0.,0.0150000000000001,0.));
#6648=CARTESIAN_POINT('',(-0.62,5.89805981832114E-17,-7.59281015471359E-17));
#6649=CARTESIAN_POINT('Origin',(0.,0.,0.));
#6650=CARTESIAN_POINT('',(-0.635,0.0150000000000001,-7.77650717458569E-17));
#6651=CARTESIAN_POINT('Origin',(0.42,0.,0.));
#6652=CARTESIAN_POINT('',(-0.42,-3.46944695195361E-18,-5.14351655641888E-17));
#6653=CARTESIAN_POINT('Origin',(0.,0.,0.));
#6654=CARTESIAN_POINT('Origin',(0.,-0.02,0.));
#6655=CARTESIAN_POINT('',(-0.3933,-0.0534000000000001,4.81653586104654E-17));
#6656=CARTESIAN_POINT('Origin',(0.,-0.0534000000000001,0.));
#6657=CARTESIAN_POINT('',(-0.41,-0.02,-5.02105187650415E-17));
#6658=CARTESIAN_POINT('Origin',(0.,-1.48,0.));
#6659=CARTESIAN_POINT('',(-0.3933,-2.9267,4.81653586104654E-17));
#6660=CARTESIAN_POINT('Origin',(0.,-2.9267,0.));
#6661=CARTESIAN_POINT('',(-0.3933,-1.48,-4.81653586104654E-17));
#6662=CARTESIAN_POINT('Origin',(0.,-2.96,0.));
#6663=CARTESIAN_POINT('',(-0.32,-3.,-3.91886975727153E-17));
#6664=CARTESIAN_POINT('Origin',(0.,-3.,0.));
#6665=CARTESIAN_POINT('',(-0.36,-2.96,-4.40872847693047E-17));
#6666=CARTESIAN_POINT('Origin',(0.,-3.,0.));
#6667=CARTESIAN_POINT('Origin',(0.173205080756888,-0.8,-0.3));
#6668=CARTESIAN_POINT('',(0.346410161513775,-0.8,0.));
#6669=CARTESIAN_POINT('',(0.173205080756888,-0.8,-0.3));
#6670=CARTESIAN_POINT('',(0.346410161513775,-0.8,0.));
#6671=CARTESIAN_POINT('',(0.173205080756888,-1.28,-0.3));
#6672=CARTESIAN_POINT('',(0.173205080756888,-0.8,-0.3));
#6673=CARTESIAN_POINT('',(0.346410161513775,-1.28,0.));
#6674=CARTESIAN_POINT('',(0.346410161513775,-1.28,0.));
#6675=CARTESIAN_POINT('',(0.346410161513775,-0.8,0.));
#6676=CARTESIAN_POINT('Origin',(-0.173205080756888,-0.8,-0.3));
#6677=CARTESIAN_POINT('',(-0.173205080756888,-0.8,-0.3));
#6678=CARTESIAN_POINT('',(0.173205080756888,-0.8,-0.3));
#6679=CARTESIAN_POINT('',(-0.173205080756888,-1.28,-0.3));
#6680=CARTESIAN_POINT('',(-0.173205080756888,-0.8,-0.3));
#6681=CARTESIAN_POINT('',(0.173205080756888,-1.28,-0.3));
#6682=CARTESIAN_POINT('Origin',(-0.346410161513775,-0.8,-5.55111512312578E-17));
#6683=CARTESIAN_POINT('',(-0.346410161513775,-0.8,-4.24230095489963E-17));
#6684=CARTESIAN_POINT('',(-0.173205080756888,-0.8,-0.3));
#6685=CARTESIAN_POINT('',(-0.346410161513775,-1.28,-5.55111512312578E-17));
#6686=CARTESIAN_POINT('',(-0.346410161513775,-0.8,-4.24230095489963E-17));
#6687=CARTESIAN_POINT('',(-0.173205080756888,-1.28,-0.3));
#6688=CARTESIAN_POINT('Origin',(-0.173205080756888,-0.8,0.3));
#6689=CARTESIAN_POINT('',(-0.173205080756888,-0.8,0.3));
#6690=CARTESIAN_POINT('',(-0.346410161513775,-0.8,-4.24230095489963E-17));
#6691=CARTESIAN_POINT('',(-0.173205080756888,-1.28,0.3));
#6692=CARTESIAN_POINT('',(-0.173205080756888,-0.8,0.3));
#6693=CARTESIAN_POINT('',(-0.346410161513775,-1.28,-4.24230095489963E-17));
#6694=CARTESIAN_POINT('Origin',(0.173205080756888,-0.8,0.3));
#6695=CARTESIAN_POINT('',(0.173205080756888,-0.8,0.3));
#6696=CARTESIAN_POINT('',(-0.173205080756888,-0.8,0.3));
#6697=CARTESIAN_POINT('',(0.173205080756888,-1.28,0.3));
#6698=CARTESIAN_POINT('',(0.173205080756888,-0.8,0.3));
#6699=CARTESIAN_POINT('',(-0.173205080756888,-1.28,0.3));
#6700=CARTESIAN_POINT('Origin',(0.346410161513775,-0.8,0.));
#6701=CARTESIAN_POINT('',(0.173205080756888,-0.8,0.3));
#6702=CARTESIAN_POINT('',(0.173205080756888,-1.28,0.3));
#6703=CARTESIAN_POINT('Origin',(0.,-0.8,-5.55111512312578E-17));
#6704=CARTESIAN_POINT('Origin',(0.,-1.28,-5.55111512312578E-17));
#6705=CARTESIAN_POINT('',(0.,0.,0.));
#6706=CARTESIAN_POINT('Origin',(0.,0.,0.));
#6707=CARTESIAN_POINT('',(-0.42,0.16,5.14351655641888E-17));
#6708=CARTESIAN_POINT('Origin',(0.,0.16,0.));
#6709=CARTESIAN_POINT('',(-0.42,0.,5.14351655641888E-17));
#6710=CARTESIAN_POINT('',(-0.42,0.,5.14351655641888E-17));
#6711=CARTESIAN_POINT('Origin',(0.,0.,0.));
#6712=CARTESIAN_POINT('Origin',(0.,0.,0.));
#6713=CARTESIAN_POINT('',(-0.8,0.16,9.79717439317883E-17));
#6714=CARTESIAN_POINT('Origin',(0.,0.16,0.));
#6715=CARTESIAN_POINT('',(-0.8,0.,9.79717439317883E-17));
#6716=CARTESIAN_POINT('',(-0.8,0.,9.79717439317883E-17));
#6717=CARTESIAN_POINT('Origin',(0.,0.,0.));
#6718=CARTESIAN_POINT('Origin',(0.,0.16,0.));
#6719=CARTESIAN_POINT('Origin',(0.,0.,0.));
#6720=CARTESIAN_POINT('',(0.,0.,0.));
#6721=CARTESIAN_POINT('Origin',(0.,0.067277284513851,0.));
#6722=CARTESIAN_POINT('',(-0.375277674973257,0.0768195421087395,0.65));
#6723=CARTESIAN_POINT('',(0.375277674973257,0.0768195421087395,0.65));
#6724=CARTESIAN_POINT('Ctrl Pts',(-0.375277674973257,0.0768195421087395,
0.65));
#6725=CARTESIAN_POINT('Ctrl Pts',(1.66533453693773E-13,-0.0315137912242439,
0.65));
#6726=CARTESIAN_POINT('Ctrl Pts',(0.375277674973257,0.0768195421087394,
0.65));
#6727=CARTESIAN_POINT('',(-0.750555349946514,0.0768195421087394,-9.19165206894919E-17));
#6728=CARTESIAN_POINT('Ctrl Pts',(-0.750555349946514,0.0768195421087394,
-9.19165206894919E-17));
#6729=CARTESIAN_POINT('Ctrl Pts',(-0.562916512459802,-0.0315137912242434,
0.325000000000144));
#6730=CARTESIAN_POINT('Ctrl Pts',(-0.375277674973257,0.0768195421087395,
0.65));
#6731=CARTESIAN_POINT('',(-0.6175,-2.77555756156289E-17,-7.5621939847349E-17));
#6732=CARTESIAN_POINT('',(-0.734027674973257,0.067277284513851,-8.98924642641573E-17));
#6733=CARTESIAN_POINT('Origin',(0.,0.,0.));
#6734=CARTESIAN_POINT('',(-0.375277674973257,0.0768195421087395,-0.65));
#6735=CARTESIAN_POINT('Ctrl Pts',(-0.375277674973257,0.0768195421087395,
-0.65));
#6736=CARTESIAN_POINT('Ctrl Pts',(-0.562916512459968,-0.0315137912242437,
-0.324999999999856));
#6737=CARTESIAN_POINT('Ctrl Pts',(-0.750555349946514,0.0768195421087395,
-9.19165206894919E-17));
#6738=CARTESIAN_POINT('',(0.375277674973257,0.0768195421087395,-0.65));
#6739=CARTESIAN_POINT('Ctrl Pts',(0.375277674973257,0.0768195421087395,
-0.65));
#6740=CARTESIAN_POINT('Ctrl Pts',(-1.66144875635155E-13,-0.0315137912242437,
-0.65));
#6741=CARTESIAN_POINT('Ctrl Pts',(-0.375277674973257,0.0768195421087395,
-0.65));
#6742=CARTESIAN_POINT('',(0.750555349946514,0.0768195421087394,0.));
#6743=CARTESIAN_POINT('Ctrl Pts',(0.750555349946514,0.0768195421087394,
0.));
#6744=CARTESIAN_POINT('Ctrl Pts',(0.562916512459802,-0.0315137912242436,
-0.325000000000144));
#6745=CARTESIAN_POINT('Ctrl Pts',(0.375277674973257,0.0768195421087395,
-0.65));
#6746=CARTESIAN_POINT('Ctrl Pts',(0.375277674973257,0.0768195421087394,
0.65));
#6747=CARTESIAN_POINT('Ctrl Pts',(0.562916512459968,-0.0315137912242439,
0.324999999999856));
#6748=CARTESIAN_POINT('Ctrl Pts',(0.750555349946514,0.0768195421087394,
0.));
#6749=CARTESIAN_POINT('Origin',(0.,0.612722715486149,0.));
#6750=CARTESIAN_POINT('',(-0.6175,0.68,-7.5621939847349E-17));
#6751=CARTESIAN_POINT('Origin',(0.,0.68,0.));
#6752=CARTESIAN_POINT('',(-0.750555349946514,0.603180457891261,-9.19165206894919E-17));
#6753=CARTESIAN_POINT('',(-0.734027674973257,0.612722715486149,-8.98924642641573E-17));
#6754=CARTESIAN_POINT('',(-0.375277674973257,0.603180457891261,0.65));
#6755=CARTESIAN_POINT('Ctrl Pts',(-0.375277674973257,0.603180457891261,
0.65));
#6756=CARTESIAN_POINT('Ctrl Pts',(-0.562916512459968,0.711513791224243,
0.324999999999856));
#6757=CARTESIAN_POINT('Ctrl Pts',(-0.750555349946514,0.603180457891261,
-9.19165206894919E-17));
#6758=CARTESIAN_POINT('',(0.375277674973257,0.603180457891261,0.65));
#6759=CARTESIAN_POINT('Ctrl Pts',(0.375277674973257,0.603180457891261,0.65));
#6760=CARTESIAN_POINT('Ctrl Pts',(-1.66755498298699E-13,0.711513791224244,
0.65));
#6761=CARTESIAN_POINT('Ctrl Pts',(-0.375277674973257,0.603180457891261,
0.65));
#6762=CARTESIAN_POINT('',(0.750555349946514,0.603180457891261,0.));
#6763=CARTESIAN_POINT('Ctrl Pts',(0.750555349946514,0.603180457891261,0.));
#6764=CARTESIAN_POINT('Ctrl Pts',(0.562916512459802,0.711513791224244,0.325000000000144));
#6765=CARTESIAN_POINT('Ctrl Pts',(0.375277674973257,0.603180457891261,0.65));
#6766=CARTESIAN_POINT('',(0.375277674973257,0.603180457891261,-0.65));
#6767=CARTESIAN_POINT('Ctrl Pts',(0.375277674973257,0.603180457891261,-0.65));
#6768=CARTESIAN_POINT('Ctrl Pts',(0.562916512459969,0.711513791224244,-0.324999999999856));
#6769=CARTESIAN_POINT('Ctrl Pts',(0.750555349946514,0.603180457891261,0.));
#6770=CARTESIAN_POINT('',(-0.375277674973257,0.603180457891261,-0.65));
#6771=CARTESIAN_POINT('Ctrl Pts',(-0.375277674973257,0.603180457891261,
-0.65));
#6772=CARTESIAN_POINT('Ctrl Pts',(1.66422431391311E-13,0.711513791224244,
-0.65));
#6773=CARTESIAN_POINT('Ctrl Pts',(0.375277674973257,0.603180457891261,-0.65));
#6774=CARTESIAN_POINT('Ctrl Pts',(-0.750555349946514,0.603180457891261,
-9.19165206894919E-17));
#6775=CARTESIAN_POINT('Ctrl Pts',(-0.562916512459802,0.711513791224244,
-0.325000000000144));
#6776=CARTESIAN_POINT('Ctrl Pts',(-0.375277674973257,0.603180457891261,
-0.65));
#6777=CARTESIAN_POINT('Origin',(0.375277674973257,0.,-0.65));
#6778=CARTESIAN_POINT('',(-0.375277674973257,0.,-0.65));
#6779=CARTESIAN_POINT('',(0.375277674973257,0.,-0.65));
#6780=CARTESIAN_POINT('Origin',(-0.375277674973257,0.,-0.65));
#6781=CARTESIAN_POINT('',(-0.750555349946514,0.,-9.19165206894919E-17));
#6782=CARTESIAN_POINT('Origin',(-0.750555349946514,0.,-9.19165206894919E-17));
#6783=CARTESIAN_POINT('',(-0.375277674973257,0.,0.65));
#6784=CARTESIAN_POINT('Origin',(0.,0.,0.));
#6785=CARTESIAN_POINT('',(-0.338975,0.68,4.15124648740974E-17));
#6786=CARTESIAN_POINT('Origin',(0.,0.68,0.));
#6787=CARTESIAN_POINT('',(-0.338975,0.,4.15124648740974E-17));
#6788=CARTESIAN_POINT('',(-0.338975,0.,4.15124648740974E-17));
#6789=CARTESIAN_POINT('Origin',(0.,0.,0.));
#6790=CARTESIAN_POINT('Origin',(-0.375277674973257,0.,0.65));
#6791=CARTESIAN_POINT('',(0.375277674973257,0.,0.65));
#6792=CARTESIAN_POINT('Origin',(0.750555349946514,0.,0.));
#6793=CARTESIAN_POINT('',(0.750555349946514,0.,0.));
#6794=CARTESIAN_POINT('Origin',(0.375277674973257,0.,0.65));
#6795=CARTESIAN_POINT('Origin',(0.,0.68,-1.11022302462516E-16));
#6796=CARTESIAN_POINT('Origin',(0.,0.,-1.11022302462516E-16));
#6797=CARTESIAN_POINT('',(0.,0.,0.));
#6798=CARTESIAN_POINT('',(0.,0.,0.));
#6799=CARTESIAN_POINT('',(0.,0.,0.));
#6800=CARTESIAN_POINT('',(0.,0.,0.));
#6801=CARTESIAN_POINT('',(0.,0.,0.));
#6802=CARTESIAN_POINT('',(0.,0.,0.));
#6803=CARTESIAN_POINT('',(0.,0.,0.));
#6804=CARTESIAN_POINT('',(0.,0.,0.));
#6805=CARTESIAN_POINT('',(0.,0.,0.));
#6806=CARTESIAN_POINT('',(0.,0.,0.));
#6807=CARTESIAN_POINT('',(0.,0.,0.));
#6808=CARTESIAN_POINT('',(0.,0.,0.));
#6809=CARTESIAN_POINT('',(-4.5,-2.6,1.8));
#6810=CARTESIAN_POINT('',(-4.5,2.6,1.8));
#6811=CARTESIAN_POINT('',(-4.5,-2.,7.));
#6812=CARTESIAN_POINT('',(-4.5,2.,7.));
#6813=CARTESIAN_POINT('',(4.5,-2.6,1.8));
#6814=CARTESIAN_POINT('',(4.5,2.6,1.8));
#6815=CARTESIAN_POINT('',(4.5,-2.,7.));
#6816=CARTESIAN_POINT('',(4.5,2.,7.));
#6817=CARTESIAN_POINT('',(-12.,0.,6.));
#6818=CARTESIAN_POINT('',(12.,0.,6.));
#6819=CARTESIAN_POINT('',(-8.,0.,6.));
#6820=CARTESIAN_POINT('',(8.,0.,6.));
#6821=CARTESIAN_POINT('',(-0.96,1.90918830920368,7.90918830920368));
#6822=CARTESIAN_POINT('',(-0.96,1.90918830920368,7.90918830920368));
#6823=CARTESIAN_POINT('',(0.8,1.90918830920368,7.90918830920368));
#6824=CARTESIAN_POINT('',(0.96,1.90918830920368,7.90918830920368));
#6825=CARTESIAN_POINT('',(-0.96,-1.90918830920368,7.90918830920368));
#6826=CARTESIAN_POINT('',(-0.96,-1.90918830920368,7.90918830920368));
#6827=CARTESIAN_POINT('',(0.8,-1.90918830920368,7.90918830920368));
#6828=CARTESIAN_POINT('',(0.96,-1.90918830920368,7.90918830920368));
#6829=CARTESIAN_POINT('',(-0.96,-1.90918830920368,4.09081169079632));
#6830=CARTESIAN_POINT('',(-0.96,-1.90918830920368,4.09081169079632));
#6831=CARTESIAN_POINT('',(0.8,-1.90918830920368,4.09081169079632));
#6832=CARTESIAN_POINT('',(0.96,-1.90918830920368,4.09081169079632));
#6833=CARTESIAN_POINT('',(-0.96,1.90918830920368,4.09081169079632));
#6834=CARTESIAN_POINT('',(-0.96,1.90918830920368,4.09081169079632));
#6835=CARTESIAN_POINT('',(0.8,1.90918830920368,4.09081169079632));
#6836=CARTESIAN_POINT('',(0.96,1.90918830920368,4.09081169079632));
#6837=UNCERTAINTY_MEASURE_WITH_UNIT(LENGTH_MEASURE(0.001),#6879,
'DISTANCE_ACCURACY_VALUE',
'Maximum model space distance between geometric entities at asserted c
onnectivities');
#6838=UNCERTAINTY_MEASURE_WITH_UNIT(LENGTH_MEASURE(0.001),#6879,
'DISTANCE_ACCURACY_VALUE',
'Maximum model space distance between geometric entities at asserted c
onnectivities');
#6839=UNCERTAINTY_MEASURE_WITH_UNIT(LENGTH_MEASURE(0.001),#6879,
'DISTANCE_ACCURACY_VALUE',
'Maximum model space distance between geometric entities at asserted c
onnectivities');
#6840=UNCERTAINTY_MEASURE_WITH_UNIT(LENGTH_MEASURE(0.001),#6879,
'DISTANCE_ACCURACY_VALUE',
'Maximum model space distance between geometric entities at asserted c
onnectivities');
#6841=UNCERTAINTY_MEASURE_WITH_UNIT(LENGTH_MEASURE(0.001),#6879,
'DISTANCE_ACCURACY_VALUE',
'Maximum model space distance between geometric entities at asserted c
onnectivities');
#6842=UNCERTAINTY_MEASURE_WITH_UNIT(LENGTH_MEASURE(0.001),#6879,
'DISTANCE_ACCURACY_VALUE',
'Maximum model space distance between geometric entities at asserted c
onnectivities');
#6843=UNCERTAINTY_MEASURE_WITH_UNIT(LENGTH_MEASURE(0.001),#6879,
'DISTANCE_ACCURACY_VALUE',
'Maximum model space distance between geometric entities at asserted c
onnectivities');
#6844=UNCERTAINTY_MEASURE_WITH_UNIT(LENGTH_MEASURE(0.001),#6879,
'DISTANCE_ACCURACY_VALUE',
'Maximum model space distance between geometric entities at asserted c
onnectivities');
#6845=UNCERTAINTY_MEASURE_WITH_UNIT(LENGTH_MEASURE(0.001),#6879,
'DISTANCE_ACCURACY_VALUE',
'Maximum model space distance between geometric entities at asserted c
onnectivities');
#6846=UNCERTAINTY_MEASURE_WITH_UNIT(LENGTH_MEASURE(0.001),#6879,
'DISTANCE_ACCURACY_VALUE',
'Maximum model space distance between geometric entities at asserted c
onnectivities');
#6847=UNCERTAINTY_MEASURE_WITH_UNIT(LENGTH_MEASURE(0.001),#6879,
'DISTANCE_ACCURACY_VALUE',
'Maximum model space distance between geometric entities at asserted c
onnectivities');
#6848=UNCERTAINTY_MEASURE_WITH_UNIT(LENGTH_MEASURE(0.001),#6879,
'DISTANCE_ACCURACY_VALUE',
'Maximum model space distance between geometric entities at asserted c
onnectivities');
#6849=UNCERTAINTY_MEASURE_WITH_UNIT(LENGTH_MEASURE(0.001),#6879,
'DISTANCE_ACCURACY_VALUE',
'Maximum model space distance between geometric entities at asserted c
onnectivities');
#6850=UNCERTAINTY_MEASURE_WITH_UNIT(LENGTH_MEASURE(0.001),#6879,
'DISTANCE_ACCURACY_VALUE',
'Maximum model space distance between geometric entities at asserted c
onnectivities');
#6851=UNCERTAINTY_MEASURE_WITH_UNIT(LENGTH_MEASURE(0.001),#6879,
'DISTANCE_ACCURACY_VALUE',
'Maximum model space distance between geometric entities at asserted c
onnectivities');
#6852=UNCERTAINTY_MEASURE_WITH_UNIT(LENGTH_MEASURE(0.001),#6879,
'DISTANCE_ACCURACY_VALUE',
'Maximum model space distance between geometric entities at asserted c
onnectivities');
#6853=UNCERTAINTY_MEASURE_WITH_UNIT(LENGTH_MEASURE(0.001),#6879,
'DISTANCE_ACCURACY_VALUE',
'Maximum model space distance between geometric entities at asserted c
onnectivities');
#6854=UNCERTAINTY_MEASURE_WITH_UNIT(LENGTH_MEASURE(0.001),#6879,
'DISTANCE_ACCURACY_VALUE',
'Maximum model space distance between geometric entities at asserted c
onnectivities');
#6855=UNCERTAINTY_MEASURE_WITH_UNIT(LENGTH_MEASURE(0.001),#6879,
'DISTANCE_ACCURACY_VALUE',
'Maximum model space distance between geometric entities at asserted c
onnectivities');
#6856=UNCERTAINTY_MEASURE_WITH_UNIT(LENGTH_MEASURE(0.001),#6879,
'DISTANCE_ACCURACY_VALUE',
'Maximum model space distance between geometric entities at asserted c
onnectivities');
#6857=UNCERTAINTY_MEASURE_WITH_UNIT(LENGTH_MEASURE(0.001),#6879,
'DISTANCE_ACCURACY_VALUE',
'Maximum model space distance between geometric entities at asserted c
onnectivities');
#6858=(
GEOMETRIC_REPRESENTATION_CONTEXT(3)
GLOBAL_UNCERTAINTY_ASSIGNED_CONTEXT((#6837))
GLOBAL_UNIT_ASSIGNED_CONTEXT((#6879,#6881,#6882))
REPRESENTATION_CONTEXT('','3D')
);
#6859=(
GEOMETRIC_REPRESENTATION_CONTEXT(3)
GLOBAL_UNCERTAINTY_ASSIGNED_CONTEXT((#6838))
GLOBAL_UNIT_ASSIGNED_CONTEXT((#6879,#6881,#6882))
REPRESENTATION_CONTEXT('','3D')
);
#6860=(
GEOMETRIC_REPRESENTATION_CONTEXT(3)
GLOBAL_UNCERTAINTY_ASSIGNED_CONTEXT((#6839))
GLOBAL_UNIT_ASSIGNED_CONTEXT((#6879,#6881,#6882))
REPRESENTATION_CONTEXT('','3D')
);
#6861=(
GEOMETRIC_REPRESENTATION_CONTEXT(3)
GLOBAL_UNCERTAINTY_ASSIGNED_CONTEXT((#6840))
GLOBAL_UNIT_ASSIGNED_CONTEXT((#6879,#6881,#6882))
REPRESENTATION_CONTEXT('','3D')
);
#6862=(
GEOMETRIC_REPRESENTATION_CONTEXT(3)
GLOBAL_UNCERTAINTY_ASSIGNED_CONTEXT((#6841))
GLOBAL_UNIT_ASSIGNED_CONTEXT((#6879,#6881,#6882))
REPRESENTATION_CONTEXT('','3D')
);
#6863=(
GEOMETRIC_REPRESENTATION_CONTEXT(3)
GLOBAL_UNCERTAINTY_ASSIGNED_CONTEXT((#6842))
GLOBAL_UNIT_ASSIGNED_CONTEXT((#6879,#6881,#6882))
REPRESENTATION_CONTEXT('','3D')
);
#6864=(
GEOMETRIC_REPRESENTATION_CONTEXT(3)
GLOBAL_UNCERTAINTY_ASSIGNED_CONTEXT((#6843))
GLOBAL_UNIT_ASSIGNED_CONTEXT((#6879,#6881,#6882))
REPRESENTATION_CONTEXT('','3D')
);
#6865=(
GEOMETRIC_REPRESENTATION_CONTEXT(3)
GLOBAL_UNCERTAINTY_ASSIGNED_CONTEXT((#6844))
GLOBAL_UNIT_ASSIGNED_CONTEXT((#6879,#6881,#6882))
REPRESENTATION_CONTEXT('','3D')
);
#6866=(
GEOMETRIC_REPRESENTATION_CONTEXT(3)
GLOBAL_UNCERTAINTY_ASSIGNED_CONTEXT((#6845))
GLOBAL_UNIT_ASSIGNED_CONTEXT((#6879,#6881,#6882))
REPRESENTATION_CONTEXT('','3D')
);
#6867=(
GEOMETRIC_REPRESENTATION_CONTEXT(3)
GLOBAL_UNCERTAINTY_ASSIGNED_CONTEXT((#6846))
GLOBAL_UNIT_ASSIGNED_CONTEXT((#6879,#6881,#6882))
REPRESENTATION_CONTEXT('','3D')
);
#6868=(
GEOMETRIC_REPRESENTATION_CONTEXT(3)
GLOBAL_UNCERTAINTY_ASSIGNED_CONTEXT((#6847))
GLOBAL_UNIT_ASSIGNED_CONTEXT((#6879,#6881,#6882))
REPRESENTATION_CONTEXT('','3D')
);
#6869=(
GEOMETRIC_REPRESENTATION_CONTEXT(3)
GLOBAL_UNCERTAINTY_ASSIGNED_CONTEXT((#6848))
GLOBAL_UNIT_ASSIGNED_CONTEXT((#6879,#6881,#6882))
REPRESENTATION_CONTEXT('','3D')
);
#6870=(
GEOMETRIC_REPRESENTATION_CONTEXT(3)
GLOBAL_UNCERTAINTY_ASSIGNED_CONTEXT((#6849))
GLOBAL_UNIT_ASSIGNED_CONTEXT((#6879,#6881,#6882))
REPRESENTATION_CONTEXT('','3D')
);
#6871=(
GEOMETRIC_REPRESENTATION_CONTEXT(3)
GLOBAL_UNCERTAINTY_ASSIGNED_CONTEXT((#6850))
GLOBAL_UNIT_ASSIGNED_CONTEXT((#6879,#6881,#6882))
REPRESENTATION_CONTEXT('','3D')
);
#6872=(
GEOMETRIC_REPRESENTATION_CONTEXT(3)
GLOBAL_UNCERTAINTY_ASSIGNED_CONTEXT((#6851))
GLOBAL_UNIT_ASSIGNED_CONTEXT((#6879,#6881,#6882))
REPRESENTATION_CONTEXT('','3D')
);
#6873=(
GEOMETRIC_REPRESENTATION_CONTEXT(3)
GLOBAL_UNCERTAINTY_ASSIGNED_CONTEXT((#6852))
GLOBAL_UNIT_ASSIGNED_CONTEXT((#6879,#6881,#6882))
REPRESENTATION_CONTEXT('','3D')
);
#6874=(
GEOMETRIC_REPRESENTATION_CONTEXT(3)
GLOBAL_UNCERTAINTY_ASSIGNED_CONTEXT((#6853))
GLOBAL_UNIT_ASSIGNED_CONTEXT((#6879,#6881,#6882))
REPRESENTATION_CONTEXT('','3D')
);
#6875=(
GEOMETRIC_REPRESENTATION_CONTEXT(3)
GLOBAL_UNCERTAINTY_ASSIGNED_CONTEXT((#6854))
GLOBAL_UNIT_ASSIGNED_CONTEXT((#6879,#6881,#6882))
REPRESENTATION_CONTEXT('','3D')
);
#6876=(
GEOMETRIC_REPRESENTATION_CONTEXT(3)
GLOBAL_UNCERTAINTY_ASSIGNED_CONTEXT((#6855))
GLOBAL_UNIT_ASSIGNED_CONTEXT((#6879,#6881,#6882))
REPRESENTATION_CONTEXT('','3D')
);
#6877=(
GEOMETRIC_REPRESENTATION_CONTEXT(3)
GLOBAL_UNCERTAINTY_ASSIGNED_CONTEXT((#6856))
GLOBAL_UNIT_ASSIGNED_CONTEXT((#6879,#6881,#6882))
REPRESENTATION_CONTEXT('','3D')
);
#6878=(
GEOMETRIC_REPRESENTATION_CONTEXT(3)
GLOBAL_UNCERTAINTY_ASSIGNED_CONTEXT((#6857))
GLOBAL_UNIT_ASSIGNED_CONTEXT((#6879,#6881,#6882))
REPRESENTATION_CONTEXT('','3D')
);
#6879=(
LENGTH_UNIT()
NAMED_UNIT(*)
SI_UNIT(.CENTI.,.METRE.)
);
#6880=(
LENGTH_UNIT()
NAMED_UNIT(*)
SI_UNIT($,.METRE.)
);
#6881=(
NAMED_UNIT(*)
PLANE_ANGLE_UNIT()
SI_UNIT($,.RADIAN.)
);
#6882=(
NAMED_UNIT(*)
SI_UNIT($,.STERADIAN.)
SOLID_ANGLE_UNIT()
);
#6883=SHAPE_DEFINITION_REPRESENTATION(#6903,#6963);
#6884=SHAPE_DEFINITION_REPRESENTATION(#6904,#6964);
#6885=SHAPE_DEFINITION_REPRESENTATION(#6905,#6965);
#6886=SHAPE_DEFINITION_REPRESENTATION(#6906,#6966);
#6887=SHAPE_DEFINITION_REPRESENTATION(#6907,#6967);
#6888=SHAPE_DEFINITION_REPRESENTATION(#6908,#6968);
#6889=SHAPE_DEFINITION_REPRESENTATION(#6909,#6969);
#6890=SHAPE_DEFINITION_REPRESENTATION(#6910,#6970);
#6891=SHAPE_DEFINITION_REPRESENTATION(#6911,#6971);
#6892=SHAPE_DEFINITION_REPRESENTATION(#6912,#6972);
#6893=SHAPE_DEFINITION_REPRESENTATION(#6913,#6973);
#6894=SHAPE_DEFINITION_REPRESENTATION(#6914,#6974);
#6895=SHAPE_DEFINITION_REPRESENTATION(#6915,#6975);
#6896=SHAPE_DEFINITION_REPRESENTATION(#6916,#6976);
#6897=SHAPE_DEFINITION_REPRESENTATION(#6917,#6977);
#6898=SHAPE_DEFINITION_REPRESENTATION(#6918,#6978);
#6899=SHAPE_DEFINITION_REPRESENTATION(#6919,#6979);
#6900=SHAPE_DEFINITION_REPRESENTATION(#6920,#6980);
#6901=SHAPE_DEFINITION_REPRESENTATION(#6921,#6981);
#6902=SHAPE_DEFINITION_REPRESENTATION(#6922,#6982);
#6903=PRODUCT_DEFINITION_SHAPE('',$,#6984);
#6904=PRODUCT_DEFINITION_SHAPE('',$,#6985);
#6905=PRODUCT_DEFINITION_SHAPE('',$,#6986);
#6906=PRODUCT_DEFINITION_SHAPE('',$,#6987);
#6907=PRODUCT_DEFINITION_SHAPE('',$,#6988);
#6908=PRODUCT_DEFINITION_SHAPE('',$,#6989);
#6909=PRODUCT_DEFINITION_SHAPE('',$,#6990);
#6910=PRODUCT_DEFINITION_SHAPE('',$,#6991);
#6911=PRODUCT_DEFINITION_SHAPE('',$,#6992);
#6912=PRODUCT_DEFINITION_SHAPE('',$,#6993);
#6913=PRODUCT_DEFINITION_SHAPE('',$,#6994);
#6914=PRODUCT_DEFINITION_SHAPE('',$,#6995);
#6915=PRODUCT_DEFINITION_SHAPE('',$,#6996);
#6916=PRODUCT_DEFINITION_SHAPE('',$,#6997);
#6917=PRODUCT_DEFINITION_SHAPE('',$,#6998);
#6918=PRODUCT_DEFINITION_SHAPE('',$,#6999);
#6919=PRODUCT_DEFINITION_SHAPE('',$,#7000);
#6920=PRODUCT_DEFINITION_SHAPE('',$,#7001);
#6921=PRODUCT_DEFINITION_SHAPE('',$,#7002);
#6922=PRODUCT_DEFINITION_SHAPE('',$,#7003);
#6923=PRODUCT_DEFINITION_SHAPE($,$,#131);
#6924=PRODUCT_DEFINITION_SHAPE($,$,#132);
#6925=PRODUCT_DEFINITION_SHAPE($,$,#133);
#6926=PRODUCT_DEFINITION_SHAPE($,$,#134);
#6927=PRODUCT_DEFINITION_SHAPE($,$,#135);
#6928=PRODUCT_DEFINITION_SHAPE($,$,#136);
#6929=PRODUCT_DEFINITION_SHAPE($,$,#137);
#6930=PRODUCT_DEFINITION_SHAPE($,$,#138);
#6931=PRODUCT_DEFINITION_SHAPE($,$,#139);
#6932=PRODUCT_DEFINITION_SHAPE($,$,#140);
#6933=PRODUCT_DEFINITION_SHAPE($,$,#141);
#6934=PRODUCT_DEFINITION_SHAPE($,$,#142);
#6935=PRODUCT_DEFINITION_SHAPE($,$,#143);
#6936=PRODUCT_DEFINITION_SHAPE($,$,#144);
#6937=PRODUCT_DEFINITION_SHAPE($,$,#145);
#6938=PRODUCT_DEFINITION_SHAPE($,$,#146);
#6939=PRODUCT_DEFINITION_SHAPE($,$,#147);
#6940=PRODUCT_DEFINITION_SHAPE($,$,#148);
#6941=PRODUCT_DEFINITION_SHAPE($,$,#149);
#6942=PRODUCT_DEFINITION_SHAPE($,$,#150);
#6943=PRODUCT_DEFINITION_SHAPE($,$,#151);
#6944=PRODUCT_DEFINITION_SHAPE($,$,#152);
#6945=PRODUCT_DEFINITION_SHAPE($,$,#153);
#6946=PRODUCT_DEFINITION_SHAPE($,$,#154);
#6947=PRODUCT_DEFINITION_SHAPE($,$,#155);
#6948=PRODUCT_DEFINITION_SHAPE($,$,#156);
#6949=PRODUCT_DEFINITION_SHAPE($,$,#157);
#6950=PRODUCT_DEFINITION_SHAPE($,$,#158);
#6951=PRODUCT_DEFINITION_SHAPE($,$,#159);
#6952=PRODUCT_DEFINITION_SHAPE($,$,#160);
#6953=PRODUCT_DEFINITION_SHAPE($,$,#161);
#6954=PRODUCT_DEFINITION_SHAPE($,$,#162);
#6955=PRODUCT_DEFINITION_SHAPE($,$,#163);
#6956=PRODUCT_DEFINITION_SHAPE($,$,#164);
#6957=PRODUCT_DEFINITION_SHAPE($,$,#165);
#6958=PRODUCT_DEFINITION_SHAPE($,$,#166);
#6959=PRODUCT_DEFINITION_SHAPE($,$,#167);
#6960=PRODUCT_DEFINITION_SHAPE($,$,#168);
#6961=PRODUCT_DEFINITION_SHAPE($,$,#169);
#6962=PRODUCT_DEFINITION_SHAPE($,$,#170);
#6963=SHAPE_REPRESENTATION('',(#4094,#4494,#4495,#4496,#4497,#4498,#4499,
#4500,#4501,#4502,#4503,#4504,#4505,#4506,#4507,#4508,#4509,#4510,#4511,
#4512,#4513,#4514,#4515,#4516,#4517,#4518,#4519,#4520,#4521,#4522,#4523,
#4524,#4525,#4526,#4527,#4528,#4529,#4530,#4531,#4532,#4533),#6858);
#6964=SHAPE_REPRESENTATION('',(#4095),#6859);
#6965=SHAPE_REPRESENTATION('',(#4114),#6860);
#6966=SHAPE_REPRESENTATION('',(#4121),#6861);
#6967=SHAPE_REPRESENTATION('',(#4128),#6862);
#6968=SHAPE_REPRESENTATION('',(#4161),#6863);
#6969=SHAPE_REPRESENTATION('',(#4186),#6864);
#6970=SHAPE_REPRESENTATION('',(#4219),#6865);
#6971=SHAPE_REPRESENTATION('',(#4244),#6866);
#6972=SHAPE_REPRESENTATION('',(#4257),#6867);
#6973=SHAPE_REPRESENTATION('',(#4282),#6868);
#6974=SHAPE_REPRESENTATION('',(#4295),#6869);
#6975=SHAPE_REPRESENTATION('',(#4320),#6870);
#6976=SHAPE_REPRESENTATION('',(#4329),#6871);
#6977=SHAPE_REPRESENTATION('',(#4353),#6872);
#6978=SHAPE_REPRESENTATION('',(#4379),#6873);
#6979=SHAPE_REPRESENTATION('',(#4419),#6874);
#6980=SHAPE_REPRESENTATION('',(#4443),#6875);
#6981=SHAPE_REPRESENTATION('',(#4469),#6876);
#6982=SHAPE_REPRESENTATION('',(#4478),#6877);
#6983=PRODUCT_DEFINITION_CONTEXT('part definition',#7045,'design');
#6984=PRODUCT_DEFINITION('PAT-080',
'PAT-080',#7004,#6983);
#6985=PRODUCT_DEFINITION('Base','Base',#7005,#6983);
#6986=PRODUCT_DEFINITION('Bonded pad','Bonded pad',#7006,
#6983);
#6987=PRODUCT_DEFINITION('Bonded pad (1)','Bonded pad (1)',#7007,
#6983);
#6988=PRODUCT_DEFINITION('Pipe support','Pipe support',#7008,
#6983);
#6989=PRODUCT_DEFINITION('Pipe clamp cap','Pipe clamp cap',#7009,
#6983);
#6990=PRODUCT_DEFINITION('Pipe support (1)','Pipe support (1)',#7010,
#6983);
#6991=PRODUCT_DEFINITION('Pipe clamp cap (1)',
'Pipe clamp cap (1)',#7011,#6983);
#6992=PRODUCT_DEFINITION('Pipe section','Pipe section',#7012,
#6983);
#6993=PRODUCT_DEFINITION('Union half A','Union half A',#7013,
#6983);
#6994=PRODUCT_DEFINITION('Pipe section (1)','Pipe section (1)',
#7014,#6983);
#6995=PRODUCT_DEFINITION('Union half B','Union half B',#7015,
#6983);
#6996=PRODUCT_DEFINITION('Union gasket','Union gasket',#7016,
#6983);
#6997=PRODUCT_DEFINITION('M5x14 Cap Screw','M5x14 Cap Screw',
#7017,#6983);
#6998=PRODUCT_DEFINITION('Cap Screw - M5x20','Cap Screw - M5x20',
#7018,#6983);
#6999=PRODUCT_DEFINITION('Pipe Elbow - 90 Degrees, 1-2 Inch Tapered Pipe Thread',
'Pipe Elbow - 90 Degrees, 1-2 Inch Tapered Pipe Thread',#7019,#6983);
#7000=PRODUCT_DEFINITION('Hex Pipe Nipple - 1-2 Inch Tapered Pipe Thread',
'Hex Pipe Nipple - 1-2 Inch Tapered Pipe Thread',#7020,#6983);
#7001=PRODUCT_DEFINITION('Cap Screw - M8x30',
'Cap Screw - M8x30',#7021,#6983);
#7002=PRODUCT_DEFINITION('Flat Washer - M8','Flat Washer - M8',
#7022,#6983);
#7003=PRODUCT_DEFINITION('Hex Nut - M8','Hex Nut - M8',#7023,
#6983);
#7004=PRODUCT_DEFINITION_FORMATION('',$,#7047);
#7005=PRODUCT_DEFINITION_FORMATION('',$,#7048);
#7006=PRODUCT_DEFINITION_FORMATION('',$,#7049);
#7007=PRODUCT_DEFINITION_FORMATION('',$,#7050);
#7008=PRODUCT_DEFINITION_FORMATION('',$,#7051);
#7009=PRODUCT_DEFINITION_FORMATION('',$,#7052);
#7010=PRODUCT_DEFINITION_FORMATION('',$,#7053);
#7011=PRODUCT_DEFINITION_FORMATION('',$,#7054);
#7012=PRODUCT_DEFINITION_FORMATION('',$,#7055);
#7013=PRODUCT_DEFINITION_FORMATION('',$,#7056);
#7014=PRODUCT_DEFINITION_FORMATION('',$,#7057);
#7015=PRODUCT_DEFINITION_FORMATION('',$,#7058);
#7016=PRODUCT_DEFINITION_FORMATION('',$,#7059);
#7017=PRODUCT_DEFINITION_FORMATION('',$,#7060);
#7018=PRODUCT_DEFINITION_FORMATION('',$,#7061);
#7019=PRODUCT_DEFINITION_FORMATION('',$,#7062);
#7020=PRODUCT_DEFINITION_FORMATION('',$,#7063);
#7021=PRODUCT_DEFINITION_FORMATION('',$,#7064);
#7022=PRODUCT_DEFINITION_FORMATION('',$,#7065);
#7023=PRODUCT_DEFINITION_FORMATION('',$,#7066);
#7024=PRODUCT_RELATED_PRODUCT_CATEGORY('PAT-080',
'PAT-080',(#7047));
#7025=PRODUCT_RELATED_PRODUCT_CATEGORY('Base','Base',(#7048));
#7026=PRODUCT_RELATED_PRODUCT_CATEGORY('Bonded pad','Bonded pad',(#7049));
#7027=PRODUCT_RELATED_PRODUCT_CATEGORY('Bonded pad (1)',
'Bonded pad (1)',(#7050));
#7028=PRODUCT_RELATED_PRODUCT_CATEGORY('Pipe support','Pipe support',(#7051));
#7029=PRODUCT_RELATED_PRODUCT_CATEGORY('Pipe clamp cap',
'Pipe clamp cap',(#7052));
#7030=PRODUCT_RELATED_PRODUCT_CATEGORY('Pipe support (1)',
'Pipe support (1)',(#7053));
#7031=PRODUCT_RELATED_PRODUCT_CATEGORY('Pipe clamp cap (1)',
'Pipe clamp cap (1)',(#7054));
#7032=PRODUCT_RELATED_PRODUCT_CATEGORY('Pipe section','Pipe section',(#7055));
#7033=PRODUCT_RELATED_PRODUCT_CATEGORY('Union half A','Union half A',(#7056));
#7034=PRODUCT_RELATED_PRODUCT_CATEGORY('Pipe section (1)',
'Pipe section (1)',(#7057));
#7035=PRODUCT_RELATED_PRODUCT_CATEGORY('Union half B','Union half B',(#7058));
#7036=PRODUCT_RELATED_PRODUCT_CATEGORY('Union gasket','Union gasket',(#7059));
#7037=PRODUCT_RELATED_PRODUCT_CATEGORY('M5x14 Cap Screw',
'M5x14 Cap Screw',(#7060));
#7038=PRODUCT_RELATED_PRODUCT_CATEGORY('Cap Screw - M5x20',
'Cap Screw - M5x20',(#7061));
#7039=PRODUCT_RELATED_PRODUCT_CATEGORY(
'Pipe Elbow - 90 Degrees, 1-2 Inch Tapered Pipe Thread',
'Pipe Elbow - 90 Degrees, 1-2 Inch Tapered Pipe Thread',(#7062));
#7040=PRODUCT_RELATED_PRODUCT_CATEGORY(
'Hex Pipe Nipple - 1-2 Inch Tapered Pipe Thread',
'Hex Pipe Nipple - 1-2 Inch Tapered Pipe Thread',(#7063));
#7041=PRODUCT_RELATED_PRODUCT_CATEGORY('Cap Screw - M8x30',
'Cap Screw - M8x30',(#7064));
#7042=PRODUCT_RELATED_PRODUCT_CATEGORY('Flat Washer - M8',
'Flat Washer - M8',(#7065));
#7043=PRODUCT_RELATED_PRODUCT_CATEGORY('Hex Nut - M8','Hex Nut - M8',(#7066));
#7044=APPLICATION_PROTOCOL_DEFINITION('international standard',
'automotive_design',2009,#7045);
#7045=APPLICATION_CONTEXT(
'Core Data for Automotive Mechanical Design Process');
#7046=PRODUCT_CONTEXT('part definition',#7045,'mechanical');
#7047=PRODUCT('PAT-080','PAT-080',
'PAT-080',(#7046));
#7048=PRODUCT('Base','Base','Base',(#7046));
#7049=PRODUCT('Bonded pad','Bonded pad','Bonded pad',(#7046));
#7050=PRODUCT('Bonded pad (1)','Bonded pad (1)','Bonded pad (1)',(#7046));
#7051=PRODUCT('Pipe support','Pipe support','Pipe support',
(#7046));
#7052=PRODUCT('Pipe clamp cap','Pipe clamp cap',
'Pipe clamp cap',(#7046));
#7053=PRODUCT('Pipe support (1)','Pipe support (1)',
'Pipe support (1)',(#7046));
#7054=PRODUCT('Pipe clamp cap (1)','Pipe clamp cap (1)',
'Pipe clamp cap (1)',(#7046));
#7055=PRODUCT('Pipe section','Pipe section','Pipe section',(#7046));
#7056=PRODUCT('Union half A','Union half A','Union half A',
(#7046));
#7057=PRODUCT('Pipe section (1)','Pipe section (1)',
'Pipe section (1)',(#7046));
#7058=PRODUCT('Union half B','Union half B','Union half B',
(#7046));
#7059=PRODUCT('Union gasket','Union gasket','Union gasket',(#7046));
#7060=PRODUCT('M5x14 Cap Screw','M5x14 Cap Screw',
'M5x14 Cap Screw',(#7046));
#7061=PRODUCT('Cap Screw - M5x20','Cap Screw - M5x20',
'Cap Screw - M5x20',(#7046));
#7062=PRODUCT('Pipe Elbow - 90 Degrees, 1-2 Inch Tapered Pipe Thread',
'Pipe Elbow - 90 Degrees, 1-2 Inch Tapered Pipe Thread',
'Pipe Elbow - 90 Degrees, 1-2 Inch Tapered Pipe Thread',(#7046));
#7063=PRODUCT('Hex Pipe Nipple - 1-2 Inch Tapered Pipe Thread',
'Hex Pipe Nipple - 1-2 Inch Tapered Pipe Thread',
'Hex Pipe Nipple - 1-2 Inch Tapered Pipe Thread',(#7046));
#7064=PRODUCT('Cap Screw - M8x30','Cap Screw - M8x30',
'Cap Screw - M8x30',(#7046));
#7065=PRODUCT('Flat Washer - M8','Flat Washer - M8',
'Flat Washer - M8',(#7046));
#7066=PRODUCT('Hex Nut - M8','Hex Nut - M8','Hex Nut - M8',
(#7046));
#7067=PRESENTATION_STYLE_ASSIGNMENT((#7072));
#7068=PRESENTATION_STYLE_ASSIGNMENT((#7073));
#7069=PRESENTATION_STYLE_ASSIGNMENT((#7074));
#7070=PRESENTATION_STYLE_ASSIGNMENT((#7075));
#7071=PRESENTATION_STYLE_ASSIGNMENT((#7076));
#7072=SURFACE_STYLE_USAGE(.BOTH.,#7077);
#7073=SURFACE_STYLE_USAGE(.BOTH.,#7078);
#7074=SURFACE_STYLE_USAGE(.BOTH.,#7079);
#7075=SURFACE_STYLE_USAGE(.BOTH.,#7080);
#7076=SURFACE_STYLE_USAGE(.BOTH.,#7081);
#7077=SURFACE_SIDE_STYLE('',(#7082));
#7078=SURFACE_SIDE_STYLE('',(#7083));
#7079=SURFACE_SIDE_STYLE('',(#7084));
#7080=SURFACE_SIDE_STYLE('',(#7085));
#7081=SURFACE_SIDE_STYLE('',(#7086));
#7082=SURFACE_STYLE_FILL_AREA(#7087);
#7083=SURFACE_STYLE_FILL_AREA(#7088);
#7084=SURFACE_STYLE_FILL_AREA(#7089);
#7085=SURFACE_STYLE_FILL_AREA(#7090);
#7086=SURFACE_STYLE_FILL_AREA(#7091);
#7087=FILL_AREA_STYLE('Steel - Satin',(#7092));
#7088=FILL_AREA_STYLE('CAD Library Painted - Deep blue',(#7093));
#7089=FILL_AREA_STYLE('CAD Library Painted - Graphite',(#7094));
#7090=FILL_AREA_STYLE('CAD Library Painted - Engineering blue',(#7095));
#7091=FILL_AREA_STYLE('CAD Library Painted - Steel gray',(#7096));
#7092=FILL_AREA_STYLE_COLOUR('Steel - Satin',#7097);
#7093=FILL_AREA_STYLE_COLOUR('CAD Library Painted - Deep blue',#7098);
#7094=FILL_AREA_STYLE_COLOUR('CAD Library Painted - Graphite',#7099);
#7095=FILL_AREA_STYLE_COLOUR('CAD Library Painted - Engineering blue',#7100);
#7096=FILL_AREA_STYLE_COLOUR('CAD Library Painted - Steel gray',#7101);
#7097=COLOUR_RGB('Steel - Satin',0.627450980392157,0.627450980392157,0.627450980392157);
#7098=COLOUR_RGB('CAD Library Painted - Deep blue',0.0784313725490196,0.203921568627451,
0.349019607843137);
#7099=COLOUR_RGB('CAD Library Painted - Graphite',0.168627450980392,0.192156862745098,
0.231372549019608);
#7100=COLOUR_RGB('CAD Library Painted - Engineering blue',0.12156862745098,
0.356862745098039,0.6);
#7101=COLOUR_RGB('CAD Library Painted - Steel gray',0.592156862745098,0.631372549019608,
0.67843137254902);
#7102=COLOUR_RGB('Dark Blue',0.08,0.2,0.34);
#7103=FILL_AREA_STYLE_COLOUR('',#7102);
#7104=FILL_AREA_STYLE('',(#7103));
#7105=SURFACE_STYLE_FILL_AREA(#7104);
#7106=SURFACE_SIDE_STYLE('',(#7105));
#7107=SURFACE_STYLE_USAGE(.BOTH.,#7106);
#7108=PRESENTATION_STYLE_ASSIGNMENT((#7107));
#7109=COLOUR_RGB('Light Blue',0.38,0.62,0.78);
#7110=FILL_AREA_STYLE_COLOUR('',#7109);
#7111=FILL_AREA_STYLE('',(#7110));
#7112=SURFACE_STYLE_FILL_AREA(#7111);
#7113=SURFACE_SIDE_STYLE('',(#7112));
#7114=SURFACE_STYLE_USAGE(.BOTH.,#7113);
#7115=PRESENTATION_STYLE_ASSIGNMENT((#7114));
#7116=COLOUR_RGB('Sky Blue',0.24,0.69,0.87);
#7117=FILL_AREA_STYLE_COLOUR('',#7116);
#7118=FILL_AREA_STYLE('',(#7117));
#7119=SURFACE_STYLE_FILL_AREA(#7118);
#7120=SURFACE_SIDE_STYLE('',(#7119));
#7121=SURFACE_STYLE_USAGE(.BOTH.,#7120);
#7122=PRESENTATION_STYLE_ASSIGNMENT((#7121));
#7123=COLOUR_RGB('Grey',0.48,0.52,0.57);
#7124=FILL_AREA_STYLE_COLOUR('',#7123);
#7125=FILL_AREA_STYLE('',(#7124));
#7126=SURFACE_STYLE_FILL_AREA(#7125);
#7127=SURFACE_SIDE_STYLE('',(#7126));
#7128=SURFACE_STYLE_USAGE(.BOTH.,#7127);
#7129=PRESENTATION_STYLE_ASSIGNMENT((#7128));
#7130=COLOUR_RGB('Black',0.12,0.14,0.17);
#7131=FILL_AREA_STYLE_COLOUR('',#7130);
#7132=FILL_AREA_STYLE('',(#7131));
#7133=SURFACE_STYLE_FILL_AREA(#7132);
#7134=SURFACE_SIDE_STYLE('',(#7133));
#7135=SURFACE_STYLE_USAGE(.BOTH.,#7134);
#7136=PRESENTATION_STYLE_ASSIGNMENT((#7135));
#7137=COLOUR_RGB('Off White',0.89,0.88,0.83);
#7138=FILL_AREA_STYLE_COLOUR('',#7137);
#7139=FILL_AREA_STYLE('',(#7138));
#7140=SURFACE_STYLE_FILL_AREA(#7139);
#7141=SURFACE_SIDE_STYLE('',(#7140));
#7142=SURFACE_STYLE_USAGE(.BOTH.,#7141);
#7143=PRESENTATION_STYLE_ASSIGNMENT((#7142));
ENDSEC;
END-ISO-10303-21;
